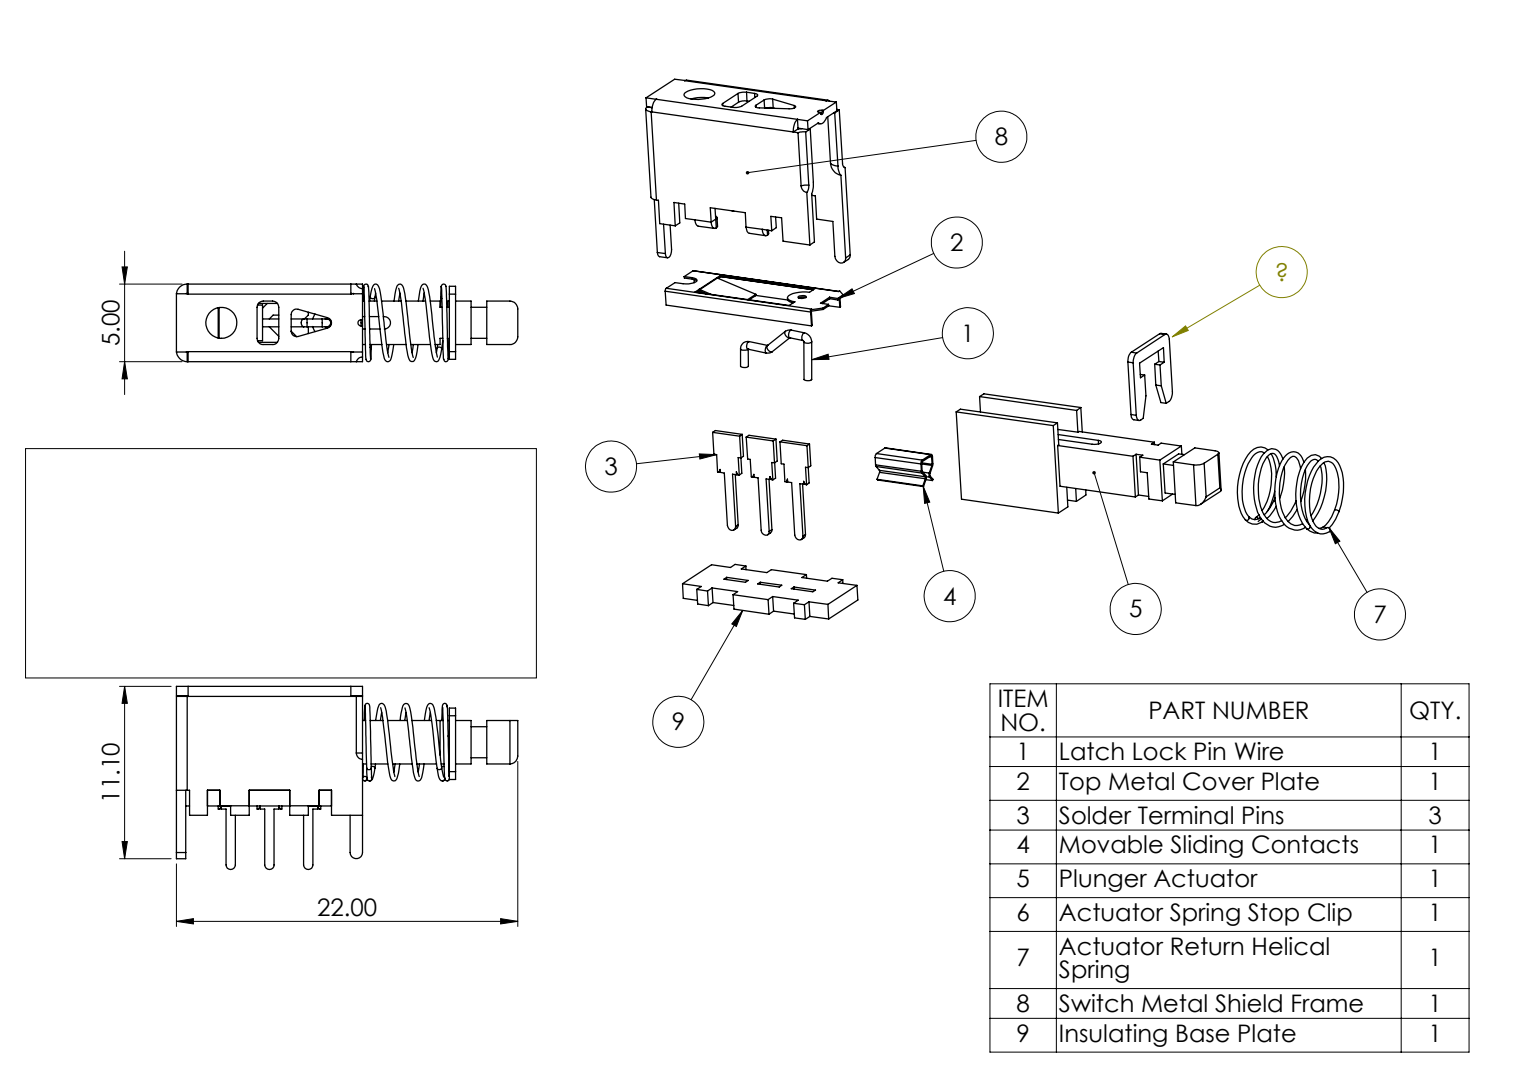
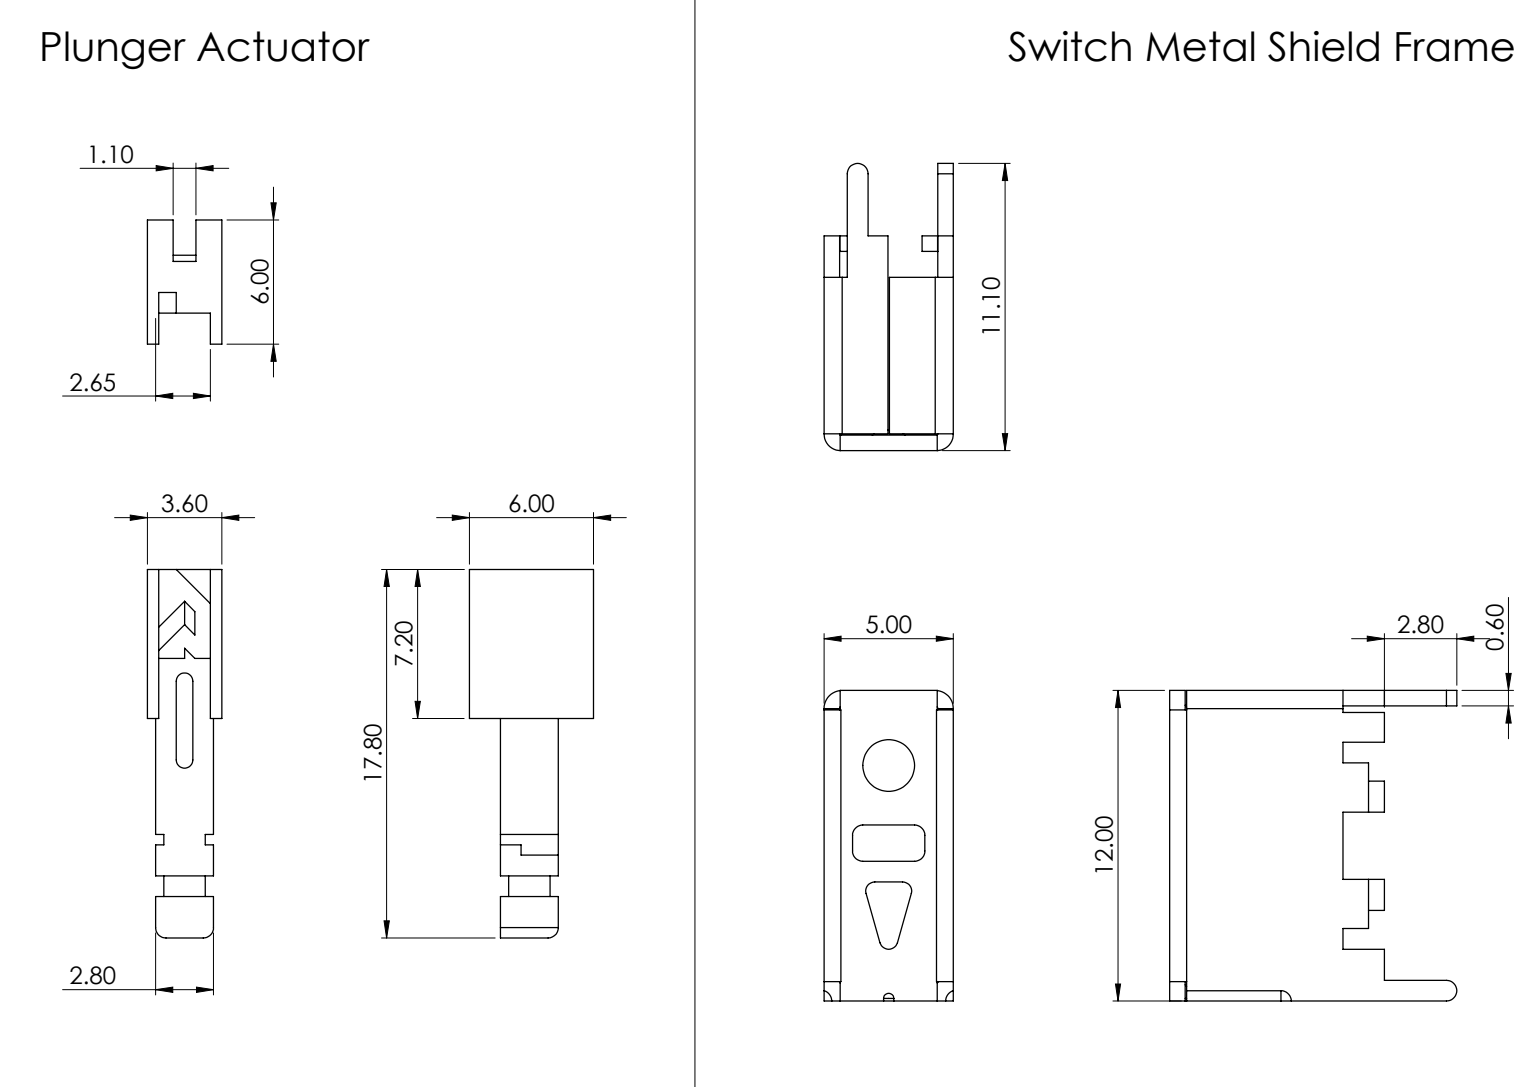
ISO-10303-21;
HEADER;
FILE_DESCRIPTION (('STEP AP214'),
    '1' );
FILE_NAME ('MAS-687',
    '2026-10-09T19:32:29',
    ( '' ),
    ( '' ),
    'SwSTEP 2.0',
    'SolidWorks 2026',
    '' );
FILE_SCHEMA (( 'AUTOMOTIVE_DESIGN' ));
ENDSEC;

DATA;
#1 = PRODUCT_DEFINITION_FORMATION_WITH_SPECIFIED_SOURCE ( 'ANY', '', #17748, .NOT_KNOWN. ) ;
#2 = ORIENTED_EDGE ( 'NONE', *, *, #12081, .F. ) ;
#3 = CARTESIAN_POINT ( 'NONE',  ( -1.670747221194380128, -5.103620102360550526, 3.047345349617600174 ) ) ;
#4 = SURFACE_STYLE_USAGE ( .BOTH. , #13787 ) ;
#5 = CARTESIAN_POINT ( 'NONE',  ( 1.315859850362970151, -5.328211948015590060, 2.737664967889629875 ) ) ;
#6 = VECTOR ( 'NONE', #12765, 1000.000000000000000 ) ;
#7 = CARTESIAN_POINT ( 'NONE',  ( 0.1749999999999999889, 2.700000000000000178, 0.5999999999999999778 ) ) ;
#8 = CARTESIAN_POINT ( 'NONE',  ( -0.4005155088301869948, -1.125163681423230200, 7.019123328904779413 ) ) ;
#9 = CYLINDRICAL_SURFACE ( 'NONE', #17623, 0.01000000000000002623 ) ;
#10 = CARTESIAN_POINT ( 'NONE',  ( -0.8934014991059870958, -4.614566048306490309, 6.877287176483410924 ) ) ;
#11 = DIRECTION ( 'NONE',  ( 1.306144734853129823E-16, -1.000000000000000000, -1.306144734853129823E-16 ) ) ;
#12 = CARTESIAN_POINT ( 'NONE',  ( 2.044452488559148851, -4.148800282540726414, 4.887392274793745273 ) ) ;
#13 = EDGE_CURVE ( 'NONE', #12197, #10130, #5306, .T. ) ;
#14 = CARTESIAN_POINT ( 'NONE',  ( -7.186903215246500006E-16, 5.131370849898470254, 6.100000000000000533 ) ) ;
#15 = EDGE_LOOP ( 'NONE', ( #13196, #1670, #3615, #581 ) ) ;
#16 = CYLINDRICAL_SURFACE ( 'NONE', #2043, 0.04999999999999969746 ) ;
#17 = EDGE_LOOP ( 'NONE', ( #524, #5810, #763, #9068 ) ) ;
#18 = CYLINDRICAL_SURFACE ( 'NONE', #7513, 0.2500000000000002220 ) ;
#19 = ORIENTED_EDGE ( 'NONE', *, *, #12813, .F. ) ;
#20 = CIRCLE ( 'NONE', #8305, 0.5000000000000000000 ) ;
#21 = CARTESIAN_POINT ( 'NONE',  ( -1.250000000000000000, 0.5999999999999999778, 7.599999999999999645 ) ) ;
#22 = EDGE_LOOP ( 'NONE', ( #588, #1750, #4383 ) ) ;
#23 = CARTESIAN_POINT ( 'NONE',  ( -1.526871680339578541, -5.259957627118655665, 3.327650196883449762 ) ) ;
#24 = CARTESIAN_POINT ( 'NONE',  ( 1.236224677598260158, -1.986830348089900777, 2.351625617688071657 ) ) ;
#25 = CARTESIAN_POINT ( 'NONE',  ( 0.3750000000000000000, 6.450000000000000178, 2.100000000000000089 ) ) ;
#26 = CARTESIAN_POINT ( 'NONE',  ( 1.652654650382400003, -0.7952867690272209522, 3.029252778805629820 ) ) ;
#27 = DIRECTION ( 'NONE',  ( 0.000000000000000000, 0.000000000000000000, -1.000000000000000000 ) ) ;
#28 = CARTESIAN_POINT ( 'NONE',  ( 0.5500000000000000444, 2.050000000000000266, 1.600000000000000089 ) ) ;
#29 = CARTESIAN_POINT ( 'NONE',  ( 1.850000000000000089, -5.599999999999999645, 6.400000000000000355 ) ) ;
#30 = AXIS2_PLACEMENT_3D ( 'NONE', #13757, #16263, #2391 ) ;
#31 = CARTESIAN_POINT ( 'NONE',  ( -1.669205944673819886, -3.147403886144329643, 6.359065158982450505 ) ) ;
#32 = CARTESIAN_POINT ( 'NONE',  ( -1.599895119336340876, -2.871785303044851023, 5.986560317183706736 ) ) ;
#33 = CARTESIAN_POINT ( 'NONE',  ( 1.821706171509118954, -0.09788135593220394226, 5.646608543709396244 ) ) ;
#34 = EDGE_CURVE ( 'NONE', #13183, #12938, #7797, .T. ) ;
#35 = CARTESIAN_POINT ( 'NONE',  ( -0.06264882350515391107, -0.4512711864406790396, 7.052569299041220319 ) ) ;
#36 = PLANE ( 'NONE',  #7974 ) ;
#37 = VERTEX_POINT ( 'NONE', #9466 ) ;
#38 = CARTESIAN_POINT ( 'NONE',  ( -2.058670345754650022, -0.2491525423728820077, 3.559656372813929881 ) ) ;
#39 = CARTESIAN_POINT ( 'NONE',  ( -0.09706517602693919000, -2.961097579838030125, 7.051451474958980725 ) ) ;
#40 = ORIENTED_EDGE ( 'NONE', *, *, #16715, .F. ) ;
#41 = DIRECTION ( 'NONE',  ( -0.7049180327868849183, 0.7092887755011130224, 8.531426931033447850E-16 ) ) ;
#42 = ORIENTED_EDGE ( 'NONE', *, *, #5974, .F. ) ;
#43 = CARTESIAN_POINT ( 'NONE',  ( 2.062913653388429136, -2.382731248990799688, 5.832754583370791224 ) ) ;
#44 = AXIS2_PLACEMENT_3D ( 'NONE', #5027, #10483, #9189 ) ;
#45 =( NAMED_UNIT ( * ) SI_UNIT ( $, .STERADIAN. ) SOLID_ANGLE_UNIT ( ) );
#46 = CARTESIAN_POINT ( 'NONE',  ( -0.6640878839024662028, -5.462076271186444565, 7.269405042592523181 ) ) ;
#47 = ORIENTED_EDGE ( 'NONE', *, *, #18282, .T. ) ;
#48 = CARTESIAN_POINT ( 'NONE',  ( 0.7109160811436110450, -1.307629111369560171, 6.943511536198400336 ) ) ;
#49 = CARTESIAN_POINT ( 'NONE',  ( 1.750316316486830059, -0.3400423728813560253, 3.126818518378580158 ) ) ;
#50 = EDGE_LOOP ( 'NONE', ( #8387, #9597, #10554, #1667 ) ) ;
#51 = PLANE ( 'NONE',  #9042 ) ;
#52 = DIRECTION ( 'NONE',  ( -2.379049338482479710E-16, 0.000000000000000000, -1.000000000000000000 ) ) ;
#53 = CARTESIAN_POINT ( 'NONE',  ( -1.883235269974520287, -3.240557039297494057, 5.517512544583926370 ) ) ;
#54 = CARTESIAN_POINT ( 'NONE',  ( 0.5500000000000000444, 6.450000000000000178, 3.399999999999999911 ) ) ;
#55 = ORIENTED_EDGE ( 'NONE', *, *, #7049, .T. ) ;
#56 = PLANE ( 'NONE',  #5985 ) ;
#57 = DIRECTION ( 'NONE',  ( 0.000000000000000000, 6.123233995736769734E-17, -1.000000000000000000 ) ) ;
#58 = CARTESIAN_POINT ( 'NONE',  ( 0.5137283630188955730, -0.4379237288135597317, 6.687652957477222770 ) ) ;
#59 = EDGE_LOOP ( 'NONE', ( #2998, #8111, #2641, #14217 ) ) ;
#60 = CARTESIAN_POINT ( 'NONE',  ( -1.440522616026439495, -4.804713230972779137, 3.241384813161591438 ) ) ;
#61 = CARTESIAN_POINT ( 'NONE',  ( -1.647941990407690627, -5.555508474576275724, 3.475676388127094896 ) ) ;
#62 = ORIENTED_EDGE ( 'NONE', *, *, #5567, .F. ) ;
#63 = FACE_OUTER_BOUND ( 'NONE', #13945, .T. ) ;
#64 = DIRECTION ( 'NONE',  ( 1.000000000000000000, 0.000000000000000000, 0.000000000000000000 ) ) ;
#65 = CARTESIAN_POINT ( 'NONE',  ( -0.5198535559317755128, -0.5906145504024216120, 2.087183161631441131 ) ) ;
#66 = ORIENTED_EDGE ( 'NONE', *, *, #5755, .T. ) ;
#67 = LINE ( 'NONE', #9878, #10862 ) ;
#68 = CARTESIAN_POINT ( 'NONE',  ( 1.097561405233190124, -1.986830348089889897, 2.618148744692249785 ) ) ;
#69 = FACE_OUTER_BOUND ( 'NONE', #15642, .T. ) ;
#70 = CARTESIAN_POINT ( 'NONE',  ( -2.039016451601939117, -3.011515032774579215, 4.939402908764104261 ) ) ;
#71 = LINE ( 'NONE', #1553, #14401 ) ;
#72 = ORIENTED_EDGE ( 'NONE', *, *, #16562, .F. ) ;
#73 = COLOUR_RGB ( '', 0.09019608, 0.27058824, 0.51372549) ;
#74 = CARTESIAN_POINT ( 'NONE',  ( 0.5500000000000000444, 6.450000000000000178, 3.200000000000000178 ) ) ;
#75 = CARTESIAN_POINT ( 'NONE',  ( -0.5609751937345790473, -0.4601694915254239682, 7.293870047334757523 ) ) ;
#76 = CARTESIAN_POINT ( 'NONE',  ( -1.145304265383870090, -3.077539021279469988, 6.755972720436099088 ) ) ;
#77 = LINE ( 'NONE', #14322, #1274 ) ;
#78 = LINE ( 'NONE', #15272, #17717 ) ;
#79 = CARTESIAN_POINT ( 'NONE',  ( -2.638803263991410741, -5.219915254237295521, 4.982085668537435730 ) ) ;
#80 = ORIENTED_EDGE ( 'NONE', *, *, #2571, .F. ) ;
#81 = ORIENTED_EDGE ( 'NONE', *, *, #13193, .F. ) ;
#82 = CARTESIAN_POINT ( 'NONE',  ( 2.500000000000000000, 10.00000000000000000, 1.600000000000000089 ) ) ;
#83 = DIRECTION ( 'NONE',  ( -1.000000000000000000, 0.000000000000000000, 0.000000000000000000 ) ) ;
#84 = VERTEX_POINT ( 'NONE', #15129 ) ;
#85 = CARTESIAN_POINT ( 'NONE',  ( 1.668426559427239608, -1.214475958216409746, 6.763847501342977075 ) ) ;
#86 = EDGE_CURVE ( 'NONE', #1835, #616, #17602, .T. ) ;
#87 = FILL_AREA_STYLE ('',( #1375 ) ) ;
#88 = AXIS2_PLACEMENT_3D ( 'NONE', #12369, #6813, #17991 ) ;
#89 = CARTESIAN_POINT ( 'NONE',  ( 0.2435295127647320035, -5.004947479095229745, 2.350795284704489507 ) ) ;
#90 = EDGE_CURVE ( 'NONE', #4403, #2448, #5018, .T. ) ;
#91 = LINE ( 'NONE', #17013, #9613 ) ;
#92 = CARTESIAN_POINT ( 'NONE',  ( -1.026235786675429917, -1.195028546288090077, 6.817920158464570335 ) ) ;
#93 = EDGE_CURVE ( 'NONE', #12376, #4659, #13727, .T. ) ;
#94 = LINE ( 'NONE', #11471, #11442 ) ;
#95 = CARTESIAN_POINT ( 'NONE',  ( 0.6150581927482109412, -4.451548030288480895, 6.971662190339319665 ) ) ;
#96 = DIRECTION ( 'NONE',  ( 6.123233995736769734E-17, 0.000000000000000000, 1.000000000000000000 ) ) ;
#97 = CARTESIAN_POINT ( 'NONE',  ( 0.8893259633308030487, -3.846052534792983923, 2.849594321892129134 ) ) ;
#98 = DIRECTION ( 'NONE',  ( -2.220446049250309876E-16, 1.000000000000000000, 0.000000000000000000 ) ) ;
#99 = ORIENTED_EDGE ( 'NONE', *, *, #10473, .T. ) ;
#100 = DIRECTION ( 'NONE',  ( 1.306144734853129823E-16, -1.000000000000000000, -1.306144734853129823E-16 ) ) ;
#101 = ORIENTED_EDGE ( 'NONE', *, *, #7303, .T. ) ;
#102 = DIRECTION ( 'NONE',  ( 0.7071067811865480168, 0.7071067811865470176, 0.000000000000000000 ) ) ;
#103 = VERTEX_POINT ( 'NONE', #12339 ) ;
#104 = CARTESIAN_POINT ( 'NONE',  ( -1.000000000000000000, -5.000000000000000000, 6.100000000000000533 ) ) ;
#105 = ADVANCED_FACE ( 'NONE', ( #14933 ), #6784, .T. ) ;
#106 = ORIENTED_EDGE ( 'NONE', *, *, #2225, .T. ) ;
#107 = CARTESIAN_POINT ( 'NONE',  ( -1.489797906646480596, -5.188771186440680694, 6.112509577910826941 ) ) ;
#108 = EDGE_CURVE ( 'NONE', #9178, #84, #9359, .T. ) ;
#109 = DIRECTION ( 'NONE',  ( -1.000000000000000000, 0.000000000000000000, 0.000000000000000000 ) ) ;
#110 = CARTESIAN_POINT ( 'NONE',  ( 2.500000000000000000, 11.15000000000000036, -1.135674796306499891E-15 ) ) ;
#111 = EDGE_CURVE ( 'NONE', #2785, #786, #2714, .T. ) ;
#112 = CARTESIAN_POINT ( 'NONE',  ( 1.889999999999999902, 7.299999999999999822, 0.5999999999999999778 ) ) ;
#113 = CARTESIAN_POINT ( 'NONE',  ( 2.500000000000000000, 2.000000000000000000, 1.600000000000000089 ) ) ;
#114 = DIRECTION ( 'NONE',  ( 0.000000000000000000, -1.000000000000000000, 0.000000000000000000 ) ) ;
#115 = CARTESIAN_POINT ( 'NONE',  ( -1.000000000000000000, -5.000000000000000000, 6.100000000000000533 ) ) ;
#116 = CARTESIAN_POINT ( 'NONE',  ( -0.09706517602693919000, -2.961097579838030125, 7.051451474958980725 ) ) ;
#117 = CARTESIAN_POINT ( 'NONE',  ( 1.978802102381368888, -3.756740257999804378, 4.152967933079626306 ) ) ;
#118 = CARTESIAN_POINT ( 'NONE',  ( 1.851073041990159984, -0.4067796610169499560, 6.153284478378259870 ) ) ;
#119 = PLANE ( 'NONE',  #9386 ) ;
#120 = DIRECTION ( 'NONE',  ( -0.000000000000000000, 1.000000000000000000, 0.000000000000000000 ) ) ;
#121 = ORIENTED_EDGE ( 'NONE', *, *, #17653, .F. ) ;
#122 = CARTESIAN_POINT ( 'NONE',  ( 0.3803919826356921829, -0.008898305084746057844, 2.682580100125298461 ) ) ;
#123 = CARTESIAN_POINT ( 'NONE',  ( -1.552749016687749783, -1.563800282540730002, 6.468535037441760061 ) ) ;
#124 = ORIENTED_EDGE ( 'NONE', *, *, #9369, .T. ) ;
#125 = ORIENTED_EDGE ( 'NONE', *, *, #6265, .F. ) ;
#126 = CARTESIAN_POINT ( 'NONE',  ( 1.236334101859160262, -3.570433951693499974, 2.697445712080690949 ) ) ;
#127 = DIRECTION ( 'NONE',  ( 1.000000000000000000, 0.000000000000000000, 0.000000000000000000 ) ) ;
#128 = CARTESIAN_POINT ( 'NONE',  ( -2.560337424259679917, -5.537711864406785978, 4.001768473655595848 ) ) ;
#129 = EDGE_CURVE ( 'NONE', #14329, #8376, #6958, .T. ) ;
#130 = ORIENTED_EDGE ( 'NONE', *, *, #2305, .T. ) ;
#131 = CARTESIAN_POINT ( 'NONE',  ( -1.432215783582709401, -0.4868644067796619179, 6.170863372171116801 ) ) ;
#132 = EDGE_LOOP ( 'NONE', ( #12967, #8164, #8169, #17199, #14235, #13899, #10080, #12493, #3954, #15631, #1582, #17423, #1346, #16815, #17146, #660 ) ) ;
#133 = PLANE ( 'NONE',  #14387 ) ;
#134 = DIRECTION ( 'NONE',  ( 0.000000000000000000, 1.000000000000000000, -2.081668171172166936E-15 ) ) ;
#135 = VECTOR ( 'NONE', #8879, 1000.000000000000000 ) ;
#136 = CARTESIAN_POINT ( 'NONE',  ( 1.854389246811829706, -2.448755237495690462, 3.819010576716856065 ) ) ;
#137 = CARTESIAN_POINT ( 'NONE',  ( 2.638803263991410741, -0.3800847457627119508, 4.982085668537405532 ) ) ;
#138 = VERTEX_POINT ( 'NONE', #2989 ) ;
#139 = LINE ( 'NONE', #14116, #7062 ) ;
#140 = CARTESIAN_POINT ( 'NONE',  ( 1.965557623688110933, -0.3889830508474575455, 5.292675575926325315 ) ) ;
#141 = ORIENTED_EDGE ( 'NONE', *, *, #4492, .T. ) ;
#142 = ORIENTED_EDGE ( 'NONE', *, *, #9998, .T. ) ;
#143 = DIRECTION ( 'NONE',  ( 0.000000000000000000, -1.000000000000000000, -1.306144734853125878E-16 ) ) ;
#144 = CARTESIAN_POINT ( 'NONE',  ( 0.05465110135556765225, -5.448728813559320372, 6.752241303418941243 ) ) ;
#145 = CARTESIAN_POINT ( 'NONE',  ( 2.011500846714318502, -0.04894067796610199889, 3.478373409938461336 ) ) ;
#146 = CARTESIAN_POINT ( 'NONE',  ( 1.791574935211219799, -5.408686440677969998, 6.226029630577610163 ) ) ;
#147 = CARTESIAN_POINT ( 'NONE',  ( -0.2097343361107079085, -0.5962015548080615845, 2.050670208512068715 ) ) ;
#148 = EDGE_CURVE ( 'NONE', #7436, #747, #4086, .T. ) ;
#149 = ORIENTED_EDGE ( 'NONE', *, *, #14001, .F. ) ;
#150 = CARTESIAN_POINT ( 'NONE',  ( 1.917298190932609891, -2.103271789531340197, 3.335187436117899917 ) ) ;
#151 = VECTOR ( 'NONE', #14058, 1000.000000000000000 ) ;
#152 = DIRECTION ( 'NONE',  ( 5.887846720064179370E-16, 1.000000000000000000, 0.000000000000000000 ) ) ;
#153 = CARTESIAN_POINT ( 'NONE',  ( -1.831349212334698828, -1.590929447188999646, 3.772065786216939554 ) ) ;
#154 = CYLINDRICAL_SURFACE ( 'NONE', #14694, 0.6500000000000003553 ) ;
#155 = EDGE_CURVE ( 'NONE', #7849, #17929, #15593, .T. ) ;
#156 = ORIENTED_EDGE ( 'NONE', *, *, #7147, .T. ) ;
#157 = CARTESIAN_POINT ( 'NONE',  ( 1.899999999999999911, 4.700000000000000178, 1.600000000000000089 ) ) ;
#158 = CARTESIAN_POINT ( 'NONE',  ( -2.020286629067959971, -0.4913135593220345210, 6.420841923842841581 ) ) ;
#159 = CARTESIAN_POINT ( 'NONE',  ( -2.283153923255329953, -3.403575057315510133, 4.129076318403500423 ) ) ;
#160 = CARTESIAN_POINT ( 'NONE',  ( -2.350000000000000089, -5.599999999999999645, 6.400000000000000355 ) ) ;
#161 = DIRECTION ( 'NONE',  ( 5.551115123125780730E-16, 1.000000000000000000, 0.000000000000000000 ) ) ;
#162 = CARTESIAN_POINT ( 'NONE',  ( -2.458531667407850563, -5.206567796610170440, 5.699238225248945966 ) ) ;
#163 = ORIENTED_EDGE ( 'NONE', *, *, #9591, .T. ) ;
#164 = EDGE_LOOP ( 'NONE', ( #16318, #961, #5589, #9306 ) ) ;
#165 = CARTESIAN_POINT ( 'NONE',  ( -2.353194804772640314, -5.224364406779659298, 4.731327187377240229 ) ) ;
#166 = DIRECTION ( 'NONE',  ( 1.000000000000000000, 1.306144734853129823E-16, 0.000000000000000000 ) ) ;
#167 = ORIENTED_EDGE ( 'NONE', *, *, #2479, .T. ) ;
#168 = CARTESIAN_POINT ( 'NONE',  ( -2.349129089426440054, -4.894025507765950245, 4.842612091679129982 ) ) ;
#169 = VECTOR ( 'NONE', #1507, 1000.000000000000000 ) ;
#170 = CARTESIAN_POINT ( 'NONE',  ( 0.6575972843460591299, -0.3612150962701959900, 2.110392115010549130 ) ) ;
#171 = CARTESIAN_POINT ( 'NONE',  ( 0.9000000000000000222, -10.00000000000000000, 6.100000000000000533 ) ) ;
#172 = CARTESIAN_POINT ( 'NONE',  ( 2.334032080503399609, -2.289578095837639715, 5.001728246382190157 ) ) ;
#173 = ADVANCED_FACE ( 'NONE', ( #18226 ), #12517, .F. ) ;
#174 = CARTESIAN_POINT ( 'NONE',  ( 1.889999999999999902, 8.500000000000000000, 0.5999999999999999778 ) ) ;
#175 = CARTESIAN_POINT ( 'NONE',  ( 1.724579595320000047, -3.939205687946140344, 3.098572228637889836 ) ) ;
#176 = DIRECTION ( 'NONE',  ( 1.000000000000000000, 0.000000000000000000, 0.000000000000000000 ) ) ;
#177 = EDGE_CURVE ( 'NONE', #9615, #14727, #5673, .T. ) ;
#178 = CARTESIAN_POINT ( 'NONE',  ( 1.835037444103841286, -4.241953435693877061, 5.620619042473564697 ) ) ;
#179 = CARTESIAN_POINT ( 'NONE',  ( -1.000000000000000000, 6.400000000000000355, 7.700000000000000178 ) ) ;
#180 = CARTESIAN_POINT ( 'NONE',  ( 2.011500846714319835, -0.3489406779661020086, 3.478373409938460448 ) ) ;
#181 = ORIENTED_EDGE ( 'NONE', *, *, #15801, .T. ) ;
#182 = CARTESIAN_POINT ( 'NONE',  ( -1.899999999999999911, 7.299999999999999822, 0.6099999999999999867 ) ) ;
#183 = ORIENTED_EDGE ( 'NONE', *, *, #8245, .T. ) ;
#184 = AXIS2_PLACEMENT_3D ( 'NONE', #11103, #16750, #840 ) ;
#185 = ADVANCED_FACE ( 'NONE', ( #9836 ), #11122, .T. ) ;
#186 = ORIENTED_EDGE ( 'NONE', *, *, #6092, .T. ) ;
#187 = EDGE_CURVE ( 'NONE', #1492, #1173, #8443, .T. ) ;
#188 = CARTESIAN_POINT ( 'NONE',  ( -2.500000000000000000, 7.299999999999999822, 1.600000000000000089 ) ) ;
#189 = CARTESIAN_POINT ( 'NONE',  ( 1.899999999999999911, 9.199999999999999289, 1.600000000000000089 ) ) ;
#190 = ORIENTED_EDGE ( 'NONE', *, *, #14281, .T. ) ;
#191 = CARTESIAN_POINT ( 'NONE',  ( 1.782460458101500889, -5.399788135593215799, 5.718585207845976015 ) ) ;
#192 = CARTESIAN_POINT ( 'NONE',  ( -0.3832714063288900630, -2.685478996738538626, 7.326064873930687504 ) ) ;
#193 = CARTESIAN_POINT ( 'NONE',  ( -1.149999999999999911, 9.248236190979499227, 7.693185165257809821 ) ) ;
#194 = CARTESIAN_POINT ( 'NONE',  ( 1.662071288245189793, -0.7952852869591279239, 3.019836320359400084 ) ) ;
#195 = CARTESIAN_POINT ( 'NONE',  ( 1.899999999999999911, 0.5999999999999999778, 6.599999999999999645 ) ) ;
#196 = CARTESIAN_POINT ( 'NONE',  ( 0.009452110982653675123, -5.000192044704546035, 2.050000000000001155 ) ) ;
#197 = CLOSED_SHELL ( 'NONE', ( #3822, #8083, #11142, #1743, #2496, #9758, #12462, #15962, #6872, #9484, #17524, #17256, #4961, #15462, #764, #3248, #10059, #5969, #10152, #4929, #18252, #3273, #16322, #10513, #3922, #2712, #13996, #6295, #532, #11967, #9528, #2422, #10741, #3839, #15384, #3945, #14577, #1473, #15447, #8798, #14553, #6473, #731, #10373, #15290, #13653, #3441, #1008, #14533, #415, #7664, #14234 ) ) ;
#198 = AXIS2_PLACEMENT_3D ( 'NONE', #9946, #12907, #5782 ) ;
#199 = EDGE_CURVE ( 'NONE', #14776, #14634, #1931, .T. ) ;
#200 = FACE_OUTER_BOUND ( 'NONE', #10573, .T. ) ;
#201 = LINE ( 'NONE', #17127, #858 ) ;
#202 = CARTESIAN_POINT ( 'NONE',  ( 2.276802572547980130, -2.495331814072260013, 4.104251954998760610 ) ) ;
#203 = CARTESIAN_POINT ( 'NONE',  ( 1.750352751699790987, -3.686875393134939394, 3.627075451280439733 ) ) ;
#204 = CARTESIAN_POINT ( 'NONE',  ( 0.1910247150515120007, -0.004449152542373194588, 2.655937705488500722 ) ) ;
#205 = EDGE_CURVE ( 'NONE', #37, #8434, #9920, .T. ) ;
#206 = DIRECTION ( 'NONE',  ( 1.142876642996489981E-16, -1.000000000000000000, -6.530723674265629391E-17 ) ) ;
#207 = EDGE_CURVE ( 'NONE', #14363, #4874, #14274, .T. ) ;
#208 = VECTOR ( 'NONE', #15083, 1000.000000000000000 ) ;
#209 = CARTESIAN_POINT ( 'NONE',  ( 1.836970198721030057E-17, 2.299999999999999822, 7.700000000000000178 ) ) ;
#210 = ORIENTED_EDGE ( 'NONE', *, *, #3477, .T. ) ;
#211 = EDGE_CURVE ( 'NONE', #3339, #16796, #8542, .T. ) ;
#212 = CARTESIAN_POINT ( 'NONE',  ( -2.043308330018790198, -0.2002118644067800157, 5.867646457774669422 ) ) ;
#213 = CARTESIAN_POINT ( 'NONE',  ( -1.881914957835490121, -1.936412895153350133, 3.286797332666350435 ) ) ;
#214 = ORIENTED_EDGE ( 'NONE', *, *, #13, .F. ) ;
#215 = EDGE_CURVE ( 'NONE', #1195, #3917, #16867, .T. ) ;
#216 = EDGE_CURVE ( 'NONE', #16860, #6769, #9644, .T. ) ;
#217 = PLANE ( 'NONE',  #15934 ) ;
#218 = AXIS2_PLACEMENT_3D ( 'NONE', #8248, #6936, #4241 ) ;
#219 = ORIENTED_EDGE ( 'NONE', *, *, #701, .F. ) ;
#220 = VECTOR ( 'NONE', #13007, 1000.000000000000000 ) ;
#221 = CARTESIAN_POINT ( 'NONE',  ( -1.644832646965619372, -4.408812330071871344, 6.383232381746490880 ) ) ;
#222 = DIRECTION ( 'NONE',  ( 0.000000000000000000, 0.000000000000000000, 1.000000000000000000 ) ) ;
#223 = CARTESIAN_POINT ( 'NONE',  ( -2.645377369053839356, -5.228813559322024851, 4.488260618344918740 ) ) ;
#224 = CIRCLE ( 'NONE', #10856, 0.09999999999999939493 ) ;
#225 = ORIENTED_EDGE ( 'NONE', *, *, #4277, .F. ) ;
#226 = CIRCLE ( 'NONE', #1107, 0.3999999999999999667 ) ;
#227 = CARTESIAN_POINT ( 'NONE',  ( 2.270487904532159984, -0.3622881355932209835, 4.080813552109670894 ) ) ;
#228 = AXIS2_PLACEMENT_3D ( 'NONE', #7610, #10199, #579 ) ;
#229 = VERTEX_POINT ( 'NONE', #1406 ) ;
#230 = DIRECTION ( 'NONE',  ( -1.000000000000000000, 1.224646799147350002E-16, 0.000000000000000000 ) ) ;
#231 = CARTESIAN_POINT ( 'NONE',  ( 0.9000000000000000222, -10.00000000000000000, 3.799999999999999822 ) ) ;
#232 = B_SPLINE_CURVE_WITH_KNOTS ( 'NONE', 3,
 ( #17325, #2928, #4655, #4553, #14218, #1537, #7186 ),
 .UNSPECIFIED., .F., .F.,
 ( 4, 1, 1, 1, 4 ),
 ( 18.06415775814129887, 18.36448856483159986, 18.49670707487869947, 18.62179267666130045, 18.84955592153880133 ),
 .UNSPECIFIED. ) ;
#233 = CARTESIAN_POINT ( 'NONE',  ( 1.810994336139499783, -2.681638120378568857, 5.667058093962681120 ) ) ;
#234 = CARTESIAN_POINT ( 'NONE',  ( -1.850000000000000089, -6.000000000000000000, 2.799999999999999822 ) ) ;
#235 = VECTOR ( 'NONE', #9014, 1000.000000000000000 ) ;
#236 = ORIENTED_EDGE ( 'NONE', *, *, #9107, .F. ) ;
#237 = VECTOR ( 'NONE', #7753, 1000.000000000000000 ) ;
#238 = PLANE ( 'NONE',  #6124 ) ;
#239 = ADVANCED_FACE ( 'NONE', ( #1597 ), #11504, .T. ) ;
#240 = VERTEX_POINT ( 'NONE', #16423 ) ;
#241 = AXIS2_PLACEMENT_3D ( 'NONE', #8801, #14538, #6201 ) ;
#242 = DIRECTION ( 'NONE',  ( -1.000000000000000000, 1.480297366166879989E-15, 7.401486830834380223E-16 ) ) ;
#243 = CARTESIAN_POINT ( 'NONE',  ( -0.5664586606772434862, -5.586652542372875452, 2.726727161522279452 ) ) ;
#244 = APPLICATION_CONTEXT ( 'automotive_design' ) ;
#245 = CARTESIAN_POINT ( 'NONE',  ( 1.750000000000000000, 11.40000000000000036, 7.700000000000000178 ) ) ;
#246 = VECTOR ( 'NONE', #2226, 1000.000000000000000 ) ;
#247 = CARTESIAN_POINT ( 'NONE',  ( 1.000896394980339332, -0.1290254237288140371, 6.829956240957368863 ) ) ;
#248 = FACE_OUTER_BOUND ( 'NONE', #10929, .T. ) ;
#249 = AXIS2_PLACEMENT_3D ( 'NONE', #9297, #17801, #8028 ) ;
#250 = LINE ( 'NONE', #4404, #4362 ) ;
#251 = CARTESIAN_POINT ( 'NONE',  ( 0.03714311608463249925, -1.078587104846649991, 7.053160869216429596 ) ) ;
#252 = EDGE_CURVE ( 'NONE', #7890, #13271, #8186, .T. ) ;
#253 = DIRECTION ( 'NONE',  ( -1.000000000000000000, -1.168655815394900078E-16, -2.220446049250309876E-16 ) ) ;
#254 = CARTESIAN_POINT ( 'NONE',  ( -0.1086361371090530797, -2.662190708450249854, 6.750146344128172160 ) ) ;
#255 = VECTOR ( 'NONE', #13621, 1000.000000000000000 ) ;
#256 = AXIS2_PLACEMENT_3D ( 'NONE', #8428, #15667, #98 ) ;
#257 = DIRECTION ( 'NONE',  ( -1.189524669241239855E-16, 1.000000000000000000, 0.000000000000000000 ) ) ;
#258 = ORIENTED_EDGE ( 'NONE', *, *, #12874, .T. ) ;
#259 = ADVANCED_FACE ( 'NONE', ( #15058 ), #2172, .T. ) ;
#260 = VECTOR ( 'NONE', #17975, 1000.000000000000000 ) ;
#261 = CARTESIAN_POINT ( 'NONE',  ( -1.850000000000000089, -6.000000000000000000, 6.899999999999999467 ) ) ;
#262 = CARTESIAN_POINT ( 'NONE',  ( -2.321479326063761395, -0.5491525423728815802, 3.414080590619972710 ) ) ;
#263 = CARTESIAN_POINT ( 'NONE',  ( -0.2564439965878500538, -4.544701183441629766, 7.039440566481220074 ) ) ;
#264 = CARTESIAN_POINT ( 'NONE',  ( -1.899999999999999911, 7.299999999999999822, 1.600000000000000089 ) ) ;
#265 = DIRECTION ( 'NONE',  ( 0.000000000000000000, 0.000000000000000000, -1.000000000000000000 ) ) ;
#266 = CARTESIAN_POINT ( 'NONE',  ( -0.6640878839024662028, -5.162076271186444743, 7.269405042592523181 ) ) ;
#267 = ORIENTED_EDGE ( 'NONE', *, *, #17989, .T. ) ;
#268 = VERTEX_POINT ( 'NONE', #877 ) ;
#269 = LINE ( 'NONE', #7559, #15424 ) ;
#270 =( NAMED_UNIT ( * ) PLANE_ANGLE_UNIT ( ) SI_UNIT ( $, .RADIAN. ) );
#271 = DIRECTION ( 'NONE',  ( -1.000000000000000000, 3.700743415417179758E-16, 0.000000000000000000 ) ) ;
#272 = ORIENTED_EDGE ( 'NONE', *, *, #15142, .T. ) ;
#273 = CARTESIAN_POINT ( 'NONE',  ( -2.461935615161759294, -1.680241723982170754, 5.690952430644365734 ) ) ;
#274 = CARTESIAN_POINT ( 'NONE',  ( -0.009452110982655128821, -0.5998079552954630467, 2.350000000000000089 ) ) ;
#275 = DIRECTION ( 'NONE',  ( -1.000000000000000000, 0.000000000000000000, 0.000000000000000000 ) ) ;
#276 = CARTESIAN_POINT ( 'NONE',  ( 1.816660071039059909, -2.429307825567370127, 6.196159040268200968 ) ) ;
#277 = CARTESIAN_POINT ( 'NONE',  ( 1.338894208872951186, -5.333856471232010676, 3.139702328019969180 ) ) ;
#278 = CARTESIAN_POINT ( 'NONE',  ( 1.864786684738361178, -0.7952867690272195089, 2.817120744449660652 ) ) ;
#279 = VECTOR ( 'NONE', #3953, 1000.000000000000000 ) ;
#280 = DIRECTION ( 'NONE',  ( 1.850371707708589879E-16, 1.000000000000000000, 0.000000000000000000 ) ) ;
#281 = DIRECTION ( 'NONE',  ( 0.000000000000000000, 1.000000000000000000, 0.000000000000000000 ) ) ;
#282 = CARTESIAN_POINT ( 'NONE',  ( -1.953802435660519921, -4.987178660919110662, 4.069478085301024173 ) ) ;
#283 = FACE_OUTER_BOUND ( 'NONE', #8177, .T. ) ;
#284 = CARTESIAN_POINT ( 'NONE',  ( -6.735557395310430190E-17, 7.000000000000000000, 6.299999999999999822 ) ) ;
#285 = EDGE_LOOP ( 'NONE', ( #13386, #1128, #2, #3206 ) ) ;
#286 = LINE ( 'NONE', #5811, #9790 ) ;
#287 = ORIENTED_EDGE ( 'NONE', *, *, #878, .F. ) ;
#288 = CARTESIAN_POINT ( 'NONE',  ( -0.1749999999999999889, 5.200000000000000178, 1.600000000000000089 ) ) ;
#289 = DIRECTION ( 'NONE',  ( -1.110223024625160090E-15, -1.000000000000000000, 0.000000000000000000 ) ) ;
#290 = EDGE_LOOP ( 'NONE', ( #11237, #4760, #6614, #15056 ) ) ;
#291 = CIRCLE ( 'NONE', #11810, 0.4000000000000001887 ) ;
#292 = CARTESIAN_POINT ( 'NONE',  ( 0.2453710345350221533, -5.444279661016954819, 6.738252723719333481 ) ) ;
#293 = CARTESIAN_POINT ( 'NONE',  ( -2.339254516529639449, -2.918361879621429011, 5.953396186326395778 ) ) ;
#294 =( LENGTH_UNIT ( ) NAMED_UNIT ( * ) SI_UNIT ( .MILLI., .METRE. ) );
#295 = FILL_AREA_STYLE_COLOUR ( '', #15889 ) ;
#296 = CARTESIAN_POINT ( 'NONE',  ( 0.1749999999999999889, 8.800000000000000711, 0.4000000000000000222 ) ) ;
#297 = DIRECTION ( 'NONE',  ( 2.242874797222539596E-16, 1.794299837778029705E-15, 1.000000000000000000 ) ) ;
#298 = DIRECTION ( 'NONE',  ( -1.000000000000000000, 1.850371707708589879E-16, 7.401486830834380223E-16 ) ) ;
#299 = CARTESIAN_POINT ( 'NONE',  ( -2.036228139452650243, -3.473439922180369788, 3.519948877554409883 ) ) ;
#300 = CARTESIAN_POINT ( 'NONE',  ( 1.942813984510739056, -1.074746228486680000, 5.363608065214415355 ) ) ;
#301 = CARTESIAN_POINT ( 'NONE',  ( 0.5664586606772286093, -0.01334745762711899916, 2.726727161522279452 ) ) ;
#302 = LINE ( 'NONE', #16960, #1412 ) ;
#303 = AXIS2_PLACEMENT_3D ( 'NONE', #18184, #4318, #5723 ) ;
#304 = CARTESIAN_POINT ( 'NONE',  ( 1.550000000000000044, -5.599999999999999645, 6.100000000000000533 ) ) ;
#305 = VERTEX_POINT ( 'NONE', #7812 ) ;
#306 = CARTESIAN_POINT ( 'NONE',  ( 2.603140590302639890, -3.873181699441240244, 5.216500493824248963 ) ) ;
#307 = CARTESIAN_POINT ( 'NONE',  ( -0.7982439214406890082, -0.1690677966101698793, 6.591424794228156081 ) ) ;
#308 = CARTESIAN_POINT ( 'NONE',  ( 1.074829861819710075, -2.285737219477669946, 2.606322265575589991 ) ) ;
#309 = EDGE_LOOP ( 'NONE', ( #17351, #15970, #6172, #13800, #4182, #16945, #17442, #3306, #8429, #9460, #10234, #6980, #680, #8084, #3687, #8931, #1239, #12150, #7376, #3119, #7225, #7211, #16942, #5389, #10768, #17470, #4563, #16616 ) ) ;
#310 = ORIENTED_EDGE ( 'NONE', *, *, #13145, .F. ) ;
#311 = CARTESIAN_POINT ( 'NONE',  ( -1.444955263746759533, -3.267686203945749490, 2.842353646881510709 ) ) ;
#312 =( LENGTH_UNIT ( ) NAMED_UNIT ( * ) SI_UNIT ( .MILLI., .METRE. ) );
#313 = CARTESIAN_POINT ( 'NONE',  ( 2.651721837666119796, -5.073093220338980025, 4.594045830208265180 ) ) ;
#314 = ORIENTED_EDGE ( 'NONE', *, *, #15602, .T. ) ;
#315 = ADVANCED_FACE ( 'NONE', ( #5219 ), #2456, .T. ) ;
#316 = FACE_OUTER_BOUND ( 'NONE', #11871, .T. ) ;
#317 = AXIS2_PLACEMENT_3D ( 'NONE', #2282, #7935, #16259 ) ;
#318 = CARTESIAN_POINT ( 'NONE',  ( -2.350067830300900162, -0.5224576271186440746, 4.825253242917699303 ) ) ;
#319 = ORIENTED_EDGE ( 'NONE', *, *, #18192, .F. ) ;
#320 = EDGE_CURVE ( 'NONE', #15780, #4246, #13459, .T. ) ;
#321 = FACE_OUTER_BOUND ( 'NONE', #2353, .T. ) ;
#322 = EDGE_CURVE ( 'NONE', #6911, #16493, #5032, .T. ) ;
#323 = CARTESIAN_POINT ( 'NONE',  ( -0.1781895581254780980, -2.146007489747939090, 2.654724878163539969 ) ) ;
#324 = EDGE_CURVE ( 'NONE', #84, #12938, #3836, .T. ) ;
#325 = CARTESIAN_POINT ( 'NONE',  ( -1.713314936023349944, -0.5610169491525430763, 3.089913064446579760 ) ) ;
#326 = ORIENTED_EDGE ( 'NONE', *, *, #6822, .T. ) ;
#327 = FACE_OUTER_BOUND ( 'NONE', #394, .T. ) ;
#328 = DIRECTION ( 'NONE',  ( 1.000000000000000000, 1.224646799147350002E-16, 0.000000000000000000 ) ) ;
#329 = CARTESIAN_POINT ( 'NONE',  ( 1.289999999999999813, 7.900000000000002132, 3.000000000000002220 ) ) ;
#330 = EDGE_LOOP ( 'NONE', ( #3061, #9828, #5549, #10787 ) ) ;
#331 = VECTOR ( 'NONE', #11702, 1000.000000000000000 ) ;
#332 = CARTESIAN_POINT ( 'NONE',  ( 0.009303514085962454744, -0.3025471796894717014, 2.316528937223512497 ) ) ;
#333 = CARTESIAN_POINT ( 'NONE',  ( -1.088937603231280304, -5.573305084745765470, 2.959627624143549074 ) ) ;
#334 = CARTESIAN_POINT ( 'NONE',  ( 1.899999999999999911, 4.700000000000000178, 0.5999999999999999778 ) ) ;
#335 = CARTESIAN_POINT ( 'NONE',  ( 1.889999999999999902, 3.500000000000000000, -7.771561172376099727E-16 ) ) ;
#336 = B_SPLINE_CURVE_WITH_KNOTS ( 'NONE', 3,
 ( #3611, #846, #9261, #16396, #652, #10551, #6486, #16212, #12146, #3518, #17765, #8602, #2858, #12943, #14328, #1649 ),
 .UNSPECIFIED., .F., .F.,
 ( 4, 1, 1, 1, 1, 1, 1, 1, 1, 1, 1, 1, 1, 4 ),
 ( 0.4999998211434338868, 0.5106244842458940170, 0.5531978902117569152, 0.5957712970451829460, 0.6383447191101619955, 0.6809180289765489613, 0.7234918990886729517, 0.7660634153087889642, 0.8086437809560700352, 0.8511815656862139479, 0.8935997744640420404, 0.9363910903531720287, 0.9718312009676199903, 1.000000000000000000 ),
 .UNSPECIFIED. ) ;
#337 = CARTESIAN_POINT ( 'NONE',  ( -1.236224677598320332, -3.613169651910099756, 2.351625617688101411 ) ) ;
#338 = ORIENTED_EDGE ( 'NONE', *, *, #2122, .F. ) ;
#339 = CARTESIAN_POINT ( 'NONE',  ( -1.219286470748949913, -1.218316834576380181, 6.712979431025680732 ) ) ;
#340 = EDGE_CURVE ( 'NONE', #11433, #9105, #9389, .T. ) ;
#341 = FACE_OUTER_BOUND ( 'NONE', #1960, .T. ) ;
#342 = CARTESIAN_POINT ( 'NONE',  ( 2.029711248330070994, -2.219713230972778728, 4.391497016172514201 ) ) ;
#343 = CARTESIAN_POINT ( 'NONE',  ( -6.735557395310420329E-17, 6.700000000000000178, 6.299999999999999822 ) ) ;
#344 = DIRECTION ( 'NONE',  ( 1.708035422500239940E-16, 1.000000000000000000, 5.978123978750840407E-16 ) ) ;
#345 = ORIENTED_EDGE ( 'NONE', *, *, #10185, .F. ) ;
#346 = CARTESIAN_POINT ( 'NONE',  ( -1.250000000000000000, 0.5999999999999999778, 6.100000000000000533 ) ) ;
#347 = CARTESIAN_POINT ( 'NONE',  ( 2.524473153133520054, -0.6128213390808875394, 3.881373716577345867 ) ) ;
#348 = CARTESIAN_POINT ( 'NONE',  ( -0.8934014991059870958, -4.614566048306490309, 6.877287176483410924 ) ) ;
#349 = CARTESIAN_POINT ( 'NONE',  ( -1.800000000000000044, 11.40000000000000036, 7.649999999999999467 ) ) ;
#350 = CARTESIAN_POINT ( 'NONE',  ( 1.850000000000000089, 0.7500000000000000000, 7.649999999999999467 ) ) ;
#351 = CARTESIAN_POINT ( 'NONE',  ( 2.351526912647309953, -5.073093220338979137, 4.606040641882800379 ) ) ;
#352 = EDGE_LOOP ( 'NONE', ( #6999, #6754, #2770, #1267 ) ) ;
#353 = ORIENTED_EDGE ( 'NONE', *, *, #5292, .T. ) ;
#354 = DIRECTION ( 'NONE',  ( 0.000000000000000000, 0.000000000000000000, 1.000000000000000000 ) ) ;
#355 = PLANE ( 'NONE',  #1395 ) ;
#356 = VERTEX_POINT ( 'NONE', #17700 ) ;
#357 = CARTESIAN_POINT ( 'NONE',  ( -1.149999999999999911, 9.274118095489749081, 7.596592582628910684 ) ) ;
#358 = CARTESIAN_POINT ( 'NONE',  ( 2.022685914314938938, -1.167899381639830203, 6.418096442297061444 ) ) ;
#359 = EDGE_CURVE ( 'NONE', #3082, #8454, #16331, .T. ) ;
#360 = CARTESIAN_POINT ( 'NONE',  ( 1.139503474074560874, -0.7471169921413568504, 2.982738323988489260 ) ) ;
#361 = CARTESIAN_POINT ( 'NONE',  ( 1.899999999999999911, 2.799999999999999822, 1.600000000000000089 ) ) ;
#362 = CARTESIAN_POINT ( 'NONE',  ( -0.3413183941262150078, -2.685478996738539958, 7.028571974690709823 ) ) ;
#363 = CARTESIAN_POINT ( 'NONE',  ( -0.02999999999999379899, 12.00000000000000000, -2.869354249208270301E-17 ) ) ;
#364 = CARTESIAN_POINT ( 'NONE',  ( -0.1785884594054470975, -1.400782264522720366, 7.347870815423047652 ) ) ;
#365 = CARTESIAN_POINT ( 'NONE',  ( 1.899999999999999911, 7.299999999999999822, 0.6099999999999999867 ) ) ;
#366 = CARTESIAN_POINT ( 'NONE',  ( 0.1608173401625761778, -4.498124606865046893, 6.746714348835997299 ) ) ;
#367 = CARTESIAN_POINT ( 'NONE',  ( -2.043308330018790198, -0.5002118644067800046, 5.867646457774669422 ) ) ;
#368 = LINE ( 'NONE', #14, #4331 ) ;
#369 = CARTESIAN_POINT ( 'NONE',  ( 0.1749999999999999889, 7.500000000000000000, 3.100000000000000089 ) ) ;
#370 = ORIENTED_EDGE ( 'NONE', *, *, #6530, .F. ) ;
#371 = DIRECTION ( 'NONE',  ( -1.000000000000000000, 0.000000000000000000, 0.000000000000000000 ) ) ;
#372 = EDGE_LOOP ( 'NONE', ( #10666, #14825, #6919, #6474 ) ) ;
#373 = PLANE ( 'NONE',  #10593 ) ;
#374 = EDGE_LOOP ( 'NONE', ( #16981, #5498, #13083, #14749 ) ) ;
#375 = VECTOR ( 'NONE', #12826, 1000.000000000000000 ) ;
#376 = CARTESIAN_POINT ( 'NONE',  ( -3.503171016405825766E-15, -5.300000000000000711, 2.649999999999998579 ) ) ;
#377 = CARTESIAN_POINT ( 'NONE',  ( -2.353343516942199898, -1.773394877135329839, 4.722803042560189901 ) ) ;
#378 = CARTESIAN_POINT ( 'NONE',  ( 0.4722227023514015687, -3.477280798540335560, 2.088464165977070408 ) ) ;
#379 = EDGE_CURVE ( 'NONE', #14325, #1999, #10215, .T. ) ;
#380 = PRESENTATION_STYLE_ASSIGNMENT (( #14351 ) ) ;
#381 =( NAMED_UNIT ( * ) SI_UNIT ( $, .STERADIAN. ) SOLID_ANGLE_UNIT ( ) );
#382 = DIRECTION ( 'NONE',  ( 1.000000000000000000, 0.000000000000000000, 0.000000000000000000 ) ) ;
#383 = CARTESIAN_POINT ( 'NONE',  ( 1.928817277882869829, -1.144611093351550091, 6.048484184565929844 ) ) ;
#384 = CARTESIAN_POINT ( 'NONE',  ( -1.600000000000000089, -3.475292999508519705E-16, 4.000000000000000000 ) ) ;
#385 = CARTESIAN_POINT ( 'NONE',  ( 1.401708661791409849, -4.358394877135329359, 6.590491606684049763 ) ) ;
#386 = CARTESIAN_POINT ( 'NONE',  ( -2.032257487115171291, -4.571830348089889640, 4.991258216523934976 ) ) ;
#387 = CARTESIAN_POINT ( 'NONE',  ( 0.009037091307169229856, -5.006769755134070188, 2.399753621991540076 ) ) ;
#388 = FACE_OUTER_BOUND ( 'NONE', #11566, .T. ) ;
#389 = VERTEX_POINT ( 'NONE', #1060 ) ;
#390 = CARTESIAN_POINT ( 'NONE',  ( 2.543624461644950152, -3.896469987729531681, 5.457025951419980814 ) ) ;
#391 = CARTESIAN_POINT ( 'NONE',  ( -2.051331987628511211, -0.2269067796610169385, 4.618035453557344461 ) ) ;
#392 = CARTESIAN_POINT ( 'NONE',  ( -2.111627294540180166, -1.889836318576769925, 3.660877362176710559 ) ) ;
#393 = ORIENTED_EDGE ( 'NONE', *, *, #5976, .T. ) ;
#394 = EDGE_LOOP ( 'NONE', ( #11957, #9883, #11083, #12392 ) ) ;
#395 = FACE_OUTER_BOUND ( 'NONE', #17771, .T. ) ;
#396 = VERTEX_POINT ( 'NONE', #6700 ) ;
#397 = CARTESIAN_POINT ( 'NONE',  ( 1.741913176380120110, -3.640298816558360517, 3.117443785062520067 ) ) ;
#398 = EDGE_CURVE ( 'NONE', #13449, #7267, #12359, .T. ) ;
#399 = SHAPE_DEFINITION_REPRESENTATION ( #9174, #16004 ) ;
#400 = CARTESIAN_POINT ( 'NONE',  ( -0.1765068388402301069, -5.153177966101685215, 7.347961541693647902 ) ) ;
#401 = EDGE_LOOP ( 'NONE', ( #12811, #11538, #1032, #13983, #10617, #10576, #15723, #6538 ) ) ;
#402 = DIRECTION ( 'NONE',  ( 0.000000000000000000, -1.000000000000000000, -1.332267629550190018E-15 ) ) ;
#403 = CARTESIAN_POINT ( 'NONE',  ( -1.925796468768790071, -0.4957627118644070130, 6.052706598917719560 ) ) ;
#404 = VERTEX_POINT ( 'NONE', #1430 ) ;
#405 = FACE_OUTER_BOUND ( 'NONE', #8642, .T. ) ;
#406 = DIRECTION ( 'NONE',  ( 1.142385477618690076E-14, -1.110223024625153952E-16, 1.000000000000000000 ) ) ;
#407 = CARTESIAN_POINT ( 'NONE',  ( 0.2047443300700049207, -2.192584066324520187, 2.657212296411530783 ) ) ;
#408 = CARTESIAN_POINT ( 'NONE',  ( 1.750000000000000000, 0.5999999999999999778, 7.700000000000000178 ) ) ;
#409 = CARTESIAN_POINT ( 'NONE',  ( 1.192209327851080136, -0.02224576271186471527, 2.329031440774910422 ) ) ;
#410 = VERTEX_POINT ( 'NONE', #11050 ) ;
#411 = DIRECTION ( 'NONE',  ( 2.220446049250309876E-16, 1.000000000000000000, -1.850371707708599740E-16 ) ) ;
#412 = VERTEX_POINT ( 'NONE', #2819 ) ;
#413 = CARTESIAN_POINT ( 'NONE',  ( 0.007090208766915150063, -0.3376261948321719886, 2.248104425785740101 ) ) ;
#414 = CARTESIAN_POINT ( 'NONE',  ( -0.3265524029357583236, -5.457627118644064801, 6.726831181542982208 ) ) ;
#415 = ADVANCED_FACE ( 'NONE', ( #12730 ), #3243, .T. ) ;
#416 = CARTESIAN_POINT ( 'NONE',  ( -1.000000000000000000, -7.000000000000000000, 5.700000000000000178 ) ) ;
#417 = EDGE_CURVE ( 'NONE', #7791, #16660, #1347, .T. ) ;
#418 = CARTESIAN_POINT ( 'NONE',  ( -1.873832970144350130, -0.2625000000000002331, 2.826167029855650270 ) ) ;
#419 = CARTESIAN_POINT ( 'NONE',  ( -2.589141052314440916, -3.287133615874059611, 5.282633936723525991 ) ) ;
#420 = ORIENTED_EDGE ( 'NONE', *, *, #10961, .F. ) ;
#421 = CARTESIAN_POINT ( 'NONE',  ( -1.167621112247339887, -2.778632149891699932, 6.743381174846780013 ) ) ;
#422 = DIRECTION ( 'NONE',  ( 0.000000000000000000, 0.000000000000000000, 1.000000000000000000 ) ) ;
#423 = PLANE ( 'NONE',  #3044 ) ;
#424 = CARTESIAN_POINT ( 'NONE',  ( -0.3429245540020551819, -1.823812330071880705, 2.675820019639910452 ) ) ;
#425 = PLANE ( 'NONE',  #7325 ) ;
#426 = ORIENTED_EDGE ( 'NONE', *, *, #18287, .T. ) ;
#427 = DIRECTION ( 'NONE',  ( -1.000000000000000000, 0.000000000000000000, 6.123233995736759873E-17 ) ) ;
#428 = CARTESIAN_POINT ( 'NONE',  ( -0.009452110982655128821, -0.5998079552954630467, 2.350000000000000089 ) ) ;
#429 = CARTESIAN_POINT ( 'NONE',  ( -2.549960444629829848, -1.544352870612421880, 3.964598460822165382 ) ) ;
#430 = VECTOR ( 'NONE', #9262, 1000.000000000000000 ) ;
#431 = FACE_OUTER_BOUND ( 'NONE', #10323, .T. ) ;
#432 = DIRECTION ( 'NONE',  ( -1.000000000000000000, 1.850371707708589879E-16, 7.401486830834380223E-16 ) ) ;
#433 = CARTESIAN_POINT ( 'NONE',  ( 0.6207106781186549904, 3.050000000000000266, 2.628553390593269423 ) ) ;
#434 = CARTESIAN_POINT ( 'NONE',  ( 2.328217775191430139, -5.081991525423729783, 5.043379051721160522 ) ) ;
#435 = VERTEX_POINT ( 'NONE', #9942 ) ;
#436 = EDGE_CURVE ( 'NONE', #3716, #6119, #18067, .T. ) ;
#437 = ORIENTED_EDGE ( 'NONE', *, *, #18165, .T. ) ;
#438 = CARTESIAN_POINT ( 'NONE',  ( 1.000000000000000000, -8.000000000000000000, 3.700000000000000178 ) ) ;
#439 = ADVANCED_FACE ( 'NONE', ( #5496 ), #3228, .T. ) ;
#440 = DIRECTION ( 'NONE',  ( 2.018587317500279868E-16, -1.000000000000000000, -1.009293658750139934E-16 ) ) ;
#441 = ORIENTED_EDGE ( 'NONE', *, *, #14504, .T. ) ;
#442 = CARTESIAN_POINT ( 'NONE',  ( 2.339254516529669647, -2.681638120378568857, 5.953396186326336270 ) ) ;
#443 = CARTESIAN_POINT ( 'NONE',  ( -1.750000000000000000, 0.5999999999999999778, 7.700000000000000178 ) ) ;
#444 = CARTESIAN_POINT ( 'NONE',  ( -0.5372984490435469551, 4.599999999999999645, 7.700000000000000178 ) ) ;
#445 = CARTESIAN_POINT ( 'NONE',  ( -0.3949552299395130417, -1.823812330071880039, 2.379923265530350385 ) ) ;
#446 = CARTESIAN_POINT ( 'NONE',  ( 1.487835687536851470, -5.028306595106930565, 2.490167689244129789 ) ) ;
#447 = CARTESIAN_POINT ( 'NONE',  ( -2.653777292528150866, -1.773394877135329839, 4.724078510415215426 ) ) ;
#448 = CARTESIAN_POINT ( 'NONE',  ( -1.850000000000000089, -6.000000000000000000, 2.299999999999999822 ) ) ;
#449 = CARTESIAN_POINT ( 'NONE',  ( -1.772995665808888788, -4.777584066324515710, 5.735078843205186239 ) ) ;
#450 = VECTOR ( 'NONE', #504, 1000.000000000000000 ) ;
#451 = DIRECTION ( 'NONE',  ( -0.2721173643531200059, -0.9622640697945191723, 0.000000000000000000 ) ) ;
#452 = ORIENTED_EDGE ( 'NONE', *, *, #9830, .T. ) ;
#453 = ADVANCED_FACE ( 'NONE', ( #10743 ), #5286, .T. ) ;
#454 = CARTESIAN_POINT ( 'NONE',  ( -0.009452110982656868748, -5.299807955295460005, 2.350000000000000089 ) ) ;
#455 = ORIENTED_EDGE ( 'NONE', *, *, #14444, .F. ) ;
#456 = CARTESIAN_POINT ( 'NONE',  ( -1.699999999999999956, 9.299999999999998934, 7.599999999999999645 ) ) ;
#457 = FACE_BOUND ( 'NONE', #15789, .T. ) ;
#458 = VERTEX_POINT ( 'NONE', #936 ) ;
#459 = CARTESIAN_POINT ( 'NONE',  ( 2.347833536521260367, -2.541908390648839777, 4.537447324629859224 ) ) ;
#460 = SURFACE_SIDE_STYLE ('',( #6019 ) ) ;
#461 = CARTESIAN_POINT ( 'NONE',  ( 1.811729841638690219, -5.341949152542369461, 3.197954009834290012 ) ) ;
#462 = CARTESIAN_POINT ( 'NONE',  ( 1.750000000000000000, 11.40000000000000036, 7.599999999999999645 ) ) ;
#463 = ADVANCED_FACE ( 'NONE', ( #6664 ), #1664, .T. ) ;
#464 = CARTESIAN_POINT ( 'NONE',  ( 2.287919158821199783, -1.051457940198389895, 5.251517552016890633 ) ) ;
#465 = CARTESIAN_POINT ( 'NONE',  ( 2.353452300571019506, -4.125511994252439862, 4.697179287168359529 ) ) ;
#466 = CARTESIAN_POINT ( 'NONE',  ( 1.688800633088581860, -0.8418633456037974971, 3.532586505616389871 ) ) ;
#467 =( REPRESENTATION_RELATIONSHIP ('NONE','NONE', #2757, #8322 ) REPRESENTATION_RELATIONSHIP_WITH_TRANSFORMATION ( #10465 )SHAPE_REPRESENTATION_RELATIONSHIP( ) );
#468 = DIRECTION ( 'NONE',  ( 6.123233995736769734E-17, 9.462128050782581713E-15, 1.000000000000000000 ) ) ;
#469 = VECTOR ( 'NONE', #13422, 1000.000000000000000 ) ;
#470 = DIRECTION ( 'NONE',  ( -6.123233995736769734E-17, -0.000000000000000000, -1.000000000000000000 ) ) ;
#471 = ORIENTED_EDGE ( 'NONE', *, *, #11105, .F. ) ;
#472 = ADVANCED_FACE ( 'NONE', ( #11019 ), #9341, .T. ) ;
#473 = CARTESIAN_POINT ( 'NONE',  ( 0.3803919826356921829, -0.3088983050847459166, 2.682580100125298461 ) ) ;
#474 = CARTESIAN_POINT ( 'NONE',  ( 0.4005155088302400634, -4.474836318576759453, 7.019123328904770531 ) ) ;
#475 = VERTEX_POINT ( 'NONE', #15390 ) ;
#476 = ORIENTED_EDGE ( 'NONE', *, *, #2348, .F. ) ;
#477 = DIRECTION ( 'NONE',  ( 0.000000000000000000, 0.000000000000000000, -1.000000000000000000 ) ) ;
#478 = ORIENTED_EDGE ( 'NONE', *, *, #1154, .F. ) ;
#479 = CARTESIAN_POINT ( 'NONE',  ( -0.2818998297622349325, -4.245794312053861042, 7.036509827384406890 ) ) ;
#480 = CARTESIAN_POINT ( 'NONE',  ( 1.031876288691629506, -5.130932203389829915, 7.145012538880298081 ) ) ;
#481 = CLOSED_SHELL ( 'NONE', ( #1105, #2707, #9593, #6776, #453, #11667, #7385, #17067, #8138, #15405, #12267, #12757, #9929, #9494, #12651, #4830, #16140, #8466, #10660, #15825, #4528, #1215, #9827, #12773, #4933, #13085, #185, #8268, #11635, #10825, #9835, #17731, #4480, #14796, #4935, #10301, #12187, #10144, #17825, #8156, #17296, #10851, #7547, #10060, #2024, #10760, #7033, #12336, #16058, #1303, #16617, #2049, #15657, #8174, #18268, #10717, #6978, #4586, #7790, #17935, #10266, #3976, #14973, #16625, #13703, #9469, #12597, #1004, #8913, #17259, #1134, #13104, #11381, #542, #2399, #8141, #3638, #14784, #10475, #11632, #17413, #6182, #5439, #4021, #637, #11519, #640, #13095, #2808, #6975, #5978, #17597, #9926, #7014, #12152, #17426, #2903, #9854, #17163, #928, #2476, #15539, #9487, #1231, #11443, #10206, #8402, #9245, #8488, #12540, #15092, #17970, #9951, #905, #10315, #7709, #12982, #2010, #8698, #15268, #13903, #15387, #5590, #1452, #4154, #7892, #3027, #13438, #2170, #8041, #6286, #15148, #12120, #173, #4067, #18029, #7347, #6752, #6683, #5308, #14678, #12014, #16384, #16822, #2892, #6701 ) ) ;
#482 = AXIS2_PLACEMENT_3D ( 'NONE', #15870, #14482, #11517 ) ;
#483 = LINE ( 'NONE', #664, #7613 ) ;
#484 = CARTESIAN_POINT ( 'NONE',  ( -2.293398556041709835, -0.5358050847457630494, 4.171956209133480975 ) ) ;
#485 = ORIENTED_EDGE ( 'NONE', *, *, #13436, .T. ) ;
#486 = CARTESIAN_POINT ( 'NONE',  ( -1.899999999999999911, 11.15000000000000036, 7.990820364436479856E-16 ) ) ;
#487 = CARTESIAN_POINT ( 'NONE',  ( 1.889999999999999902, 4.100000000000000533, -6.512531667206379696E-16 ) ) ;
#488 = CARTESIAN_POINT ( 'NONE',  ( -1.937109463115380903, -3.426863345603793576, 4.019920026366796684 ) ) ;
#489 = CARTESIAN_POINT ( 'NONE',  ( -1.666450993087168930, -0.4824152542372879826, 6.765380371283871597 ) ) ;
#490 = VERTEX_POINT ( 'NONE', #3889 ) ;
#491 = LINE ( 'NONE', #17068, #7903 ) ;
#492 = CIRCLE ( 'NONE', #4337, 0.5999999999999998668 ) ;
#493 = EDGE_LOOP ( 'NONE', ( #3979, #4841, #1424, #2607 ) ) ;
#494 = CARTESIAN_POINT ( 'NONE',  ( -0.009227126607029439292, -0.5962421434521730790, 2.310024366371980165 ) ) ;
#495 = CARTESIAN_POINT ( 'NONE',  ( 0.06264882350516240428, -5.448728813559320372, 7.052569299041220319 ) ) ;
#496 = CARTESIAN_POINT ( 'NONE',  ( -1.811729841638699767, -0.2580508474576270195, 3.197954009834300226 ) ) ;
#497 = VECTOR ( 'NONE', #10509, 1000.000000000000000 ) ;
#498 = CARTESIAN_POINT ( 'NONE',  ( 1.155768864438629695, -4.404971453711897134, 7.088998121597438029 ) ) ;
#499 = ORIENTED_EDGE ( 'NONE', *, *, #14133, .T. ) ;
#500 = CARTESIAN_POINT ( 'NONE',  ( 2.334032080503399609, -2.289578095837639715, 5.001728246382190157 ) ) ;
#501 = AXIS2_PLACEMENT_3D ( 'NONE', #17888, #13465, #603 ) ;
#502 = CARTESIAN_POINT ( 'NONE',  ( 1.899999999999999911, 9.199999999999999289, 0.6099999999999999867 ) ) ;
#503 = AXIS2_PLACEMENT_3D ( 'NONE', #7453, #4395, #3187 ) ;
#504 = DIRECTION ( 'NONE',  ( 5.551115123125779621E-17, 0.000000000000000000, 1.000000000000000000 ) ) ;
#505 = CARTESIAN_POINT ( 'NONE',  ( 0.7368491673939637776, -3.523857375116919322, 2.783765372628159263 ) ) ;
#506 = DIRECTION ( 'NONE',  ( 1.000000000000000000, 1.283953296258166085E-32, -6.123233995736769734E-17 ) ) ;
#507 = CARTESIAN_POINT ( 'NONE',  ( -0.3750000000000000000, 3.050000000000000266, 2.100000000000000089 ) ) ;
#508 = CARTESIAN_POINT ( 'NONE',  ( 0.4114611322411816374, -1.032010528270079330, 6.711368086473216366 ) ) ;
#509 = ORIENTED_EDGE ( 'NONE', *, *, #12081, .T. ) ;
#510 = EDGE_CURVE ( 'NONE', #2436, #16660, #16741, .T. ) ;
#511 = AXIS2_PLACEMENT_3D ( 'NONE', #3068, #18227, #15681 ) ;
#512 = CARTESIAN_POINT ( 'NONE',  ( 1.800000000000000044, 11.40000000000000036, 1.600000000000000089 ) ) ;
#513 = CIRCLE ( 'NONE', #1410, 0.2500000000000002220 ) ;
#514 = VECTOR ( 'NONE', #10308, 1000.000000000000000 ) ;
#515 = DIRECTION ( 'NONE',  ( 1.059337802663170094E-14, 1.000000000000000000, 1.929541063032960169E-30 ) ) ;
#516 = CARTESIAN_POINT ( 'NONE',  ( 0.7756407636289058827, -1.008722239981790558, 7.238010066725317770 ) ) ;
#517 = EDGE_LOOP ( 'NONE', ( #11060, #3583, #4007, #16442 ) ) ;
#518 = DIRECTION ( 'NONE',  ( -2.337311630789800155E-16, 1.000000000000000000, 0.000000000000000000 ) ) ;
#519 = DIRECTION ( 'NONE',  ( 1.000000000000000000, -1.103950578158349959E-14, 0.000000000000000000 ) ) ;
#520 = CARTESIAN_POINT ( 'NONE',  ( 1.550000000000000044, -6.000000000000000000, 5.100000000000000533 ) ) ;
#521 = CARTESIAN_POINT ( 'NONE',  ( 1.477796163681079911, -5.117584745762710163, 6.531563725478140015 ) ) ;
#522 = ORIENTED_EDGE ( 'NONE', *, *, #6504, .F. ) ;
#523 = VECTOR ( 'NONE', #3659, 1000.000000000000000 ) ;
#524 = ORIENTED_EDGE ( 'NONE', *, *, #10146, .F. ) ;
#525 = CARTESIAN_POINT ( 'NONE',  ( 2.500000000000000000, 10.00000000000000000, -5.075305255429290705E-16 ) ) ;
#526 = DIRECTION ( 'NONE',  ( -2.220446049250309876E-16, -1.000000000000000000, 4.930380657631319405E-32 ) ) ;
#527 = ORIENTED_EDGE ( 'NONE', *, *, #3623, .T. ) ;
#528 = EDGE_CURVE ( 'NONE', #17501, #10555, #13235, .T. ) ;
#529 = AXIS2_PLACEMENT_3D ( 'NONE', #9899, #3969, #6850 ) ;
#530 = CARTESIAN_POINT ( 'NONE',  ( -0.1110902655589390137, -2.961097579838030569, 7.351560417169478612 ) ) ;
#531 = VECTOR ( 'NONE', #12503, 1000.000000000000000 ) ;
#532 = ADVANCED_FACE ( 'NONE', ( #12413 ), #10936, .F. ) ;
#533 = LINE ( 'NONE', #14427, #12662 ) ;
#534 = CARTESIAN_POINT ( 'NONE',  ( 2.500000000000000000, 9.199999999999999289, 1.600000000000000089 ) ) ;
#535 = CARTESIAN_POINT ( 'NONE',  ( 2.036228139452630259, -2.126560077819629857, 3.519948877554369915 ) ) ;
#536 = EDGE_CURVE ( 'NONE', #3882, #3854, #4603, .T. ) ;
#537 = CARTESIAN_POINT ( 'NONE',  ( -0.1749999999999999889, 8.200000000000001066, 0.4000000000000000222 ) ) ;
#538 = AXIS2_PLACEMENT_3D ( 'NONE', #1149, #15052, #18243 ) ;
#539 = CARTESIAN_POINT ( 'NONE',  ( -2.161802606005209793, -5.010466949207389220, 3.769755311421840283 ) ) ;
#540 = EDGE_CURVE ( 'NONE', #10260, #6008, #5380, .T. ) ;
#541 = CARTESIAN_POINT ( 'NONE',  ( 1.399999999999999911, -5.500000000000000000, 5.100000000000000533 ) ) ;
#542 = ADVANCED_FACE ( 'NONE', ( #18116 ), #8251, .F. ) ;
#543 = VECTOR ( 'NONE', #1826, 1000.000000000000000 ) ;
#544 = VECTOR ( 'NONE', #5083, 1000.000000000000000 ) ;
#545 = DIRECTION ( 'NONE',  ( -4.440892098500630106E-16, 0.000000000000000000, 1.000000000000000000 ) ) ;
#546 = EDGE_LOOP ( 'NONE', ( #14496, #12522, #5384, #16838 ) ) ;
#547 = VECTOR ( 'NONE', #6134, 1000.000000000000000 ) ;
#548 = FACE_OUTER_BOUND ( 'NONE', #2723, .T. ) ;
#549 = ORIENTED_EDGE ( 'NONE', *, *, #17371, .T. ) ;
#550 = DIRECTION ( 'NONE',  ( -1.000000000000000000, -8.881784197001249119E-17, -1.776356839400249824E-16 ) ) ;
#551 = DIRECTION ( 'NONE',  ( 0.000000000000000000, -1.000000000000000000, 0.000000000000000000 ) ) ;
#552 =( GEOMETRIC_REPRESENTATION_CONTEXT ( 3 ) GLOBAL_UNCERTAINTY_ASSIGNED_CONTEXT ( ( #2517 ) ) GLOBAL_UNIT_ASSIGNED_CONTEXT ( ( #4504, #3040, #6174 ) ) REPRESENTATION_CONTEXT ( 'NONE', 'WORKASPACE' ) );
#553 = ORIENTED_EDGE ( 'NONE', *, *, #10570, .F. ) ;
#554 = DIRECTION ( 'NONE',  ( 1.306144734853129823E-16, -1.000000000000000000, -6.530723674265629391E-17 ) ) ;
#555 = CARTESIAN_POINT ( 'NONE',  ( 0.4539185741479240255, -2.215872354612800521, 2.390735265170440105 ) ) ;
#556 = EDGE_CURVE ( 'NONE', #14368, #9144, #15286, .T. ) ;
#557 = SPHERICAL_SURFACE ( 'NONE', #241, 0.8000000000000000444 ) ;
#558 = CARTESIAN_POINT ( 'NONE',  ( -2.500000000000000000, 10.00000000000000000, 1.600000000000000089 ) ) ;
#559 = VECTOR ( 'NONE', #7948, 1000.000000000000000 ) ;
#560 = FACE_BOUND ( 'NONE', #795, .T. ) ;
#561 = ADVANCED_FACE ( 'NONE', ( #4065 ), #6855, .F. ) ;
#562 = FACE_OUTER_BOUND ( 'NONE', #15, .T. ) ;
#563 = CARTESIAN_POINT ( 'NONE',  ( 0.4005155088302400634, -4.474836318576759453, 7.019123328904770531 ) ) ;
#564 = CARTESIAN_POINT ( 'NONE',  ( 2.050994839075679366, -0.9815930753335269099, 4.608774933727144862 ) ) ;
#565 = CARTESIAN_POINT ( 'NONE',  ( 0.8731223871105069367, -0.1290254237288140371, 6.558046933601105799 ) ) ;
#566 = CARTESIAN_POINT ( 'NONE',  ( 2.500000000000000000, 4.700000000000000178, 1.600000000000000089 ) ) ;
#567 = DIRECTION ( 'NONE',  ( 0.000000000000000000, 0.000000000000000000, -1.000000000000000000 ) ) ;
#568 = ORIENTED_EDGE ( 'NONE', *, *, #93, .F. ) ;
#569 = CARTESIAN_POINT ( 'NONE',  ( -0.9707742057416274273, -0.1735169491525429541, 6.508944043303927174 ) ) ;
#570 = CARTESIAN_POINT ( 'NONE',  ( -2.351999299633229956, -3.333710192450639820, 4.782734406438290620 ) ) ;
#571 = ORIENTED_EDGE ( 'NONE', *, *, #11074, .T. ) ;
#572 = AXIS2_PLACEMENT_3D ( 'NONE', #3697, #17666, #14917 ) ;
#573 = ORIENTED_EDGE ( 'NONE', *, *, #11966, .T. ) ;
#574 = CARTESIAN_POINT ( 'NONE',  ( 2.616666666666669805, -6.661338147750939243E-16, 7.649999999999999467 ) ) ;
#575 = ORIENTED_EDGE ( 'NONE', *, *, #10898, .F. ) ;
#576 = FACE_OUTER_BOUND ( 'NONE', #11007, .T. ) ;
#577 = ITEM_DEFINED_TRANSFORMATION ( 'NONE', 'NONE', #8257,  #17681 ) ;
#578 = CARTESIAN_POINT ( 'NONE',  ( -1.610878918935079840, -5.568855932203385706, 2.590989782159090815 ) ) ;
#579 = DIRECTION ( 'NONE',  ( 1.000000000000000000, 0.000000000000000000, 0.000000000000000000 ) ) ;
#580 = CARTESIAN_POINT ( 'NONE',  ( 2.306642602145299925, -0.3845338983050849979, 5.166805192608480368 ) ) ;
#581 = ORIENTED_EDGE ( 'NONE', *, *, #8066, .F. ) ;
#582 = EDGE_CURVE ( 'NONE', #14617, #14203, #6481, .T. ) ;
#583 = DIRECTION ( 'NONE',  ( 0.000000000000000000, 1.000000000000000000, 0.000000000000000000 ) ) ;
#584 = FACE_BOUND ( 'NONE', #16591, .T. ) ;
#585 = VECTOR ( 'NONE', #11479, 1000.000000000000000 ) ;
#586 = CARTESIAN_POINT ( 'NONE',  ( 1.974086094277279768, -4.195376859117311064, 5.263813741415705572 ) ) ;
#587 = CARTESIAN_POINT ( 'NONE',  ( 1.554165089654128584, -0.1201271186440679706, 6.851145244874527584 ) ) ;
#588 = ORIENTED_EDGE ( 'NONE', *, *, #1576, .T. ) ;
#589 = ORIENTED_EDGE ( 'NONE', *, *, #4710, .F. ) ;
#590 = CARTESIAN_POINT ( 'NONE',  ( -2.431060148753501515, -0.5447033898305090327, 3.635668498923334102 ) ) ;
#591 = ORIENTED_EDGE ( 'NONE', *, *, #1780, .F. ) ;
#592 = CARTESIAN_POINT ( 'NONE',  ( 1.828929293328490072E-16, 2.399999999999999911, 5.100000000000000533 ) ) ;
#593 = CARTESIAN_POINT ( 'NONE',  ( -1.800000000000000044, 12.00000000000000000, 1.600000000000000089 ) ) ;
#594 = DIRECTION ( 'NONE',  ( -6.476300976980080477E-16, 9.251858538542978977E-17, -1.000000000000000000 ) ) ;
#595 = AXIS2_PLACEMENT_3D ( 'NONE', #12279, #13477, #898 ) ;
#596 = CARTESIAN_POINT ( 'NONE',  ( 2.642175029090480631, -4.102223705964154199, 4.450952196049445142 ) ) ;
#597 = ORIENTED_EDGE ( 'NONE', *, *, #12740, .F. ) ;
#598 = ADVANCED_FACE ( 'NONE', ( #11204 ), #1488, .T. ) ;
#599 = CARTESIAN_POINT ( 'NONE',  ( 2.295719155670170153, -2.312866384125930264, 5.218091927917190453 ) ) ;
#600 = CARTESIAN_POINT ( 'NONE',  ( 2.500000000000000000, 11.25000000000000000, 7.649999999999999467 ) ) ;
#601 = CARTESIAN_POINT ( 'NONE',  ( 5.829811056852189859E-17, 3.957026083511942627, 8.102080397533576672 ) ) ;
#602 = CARTESIAN_POINT ( 'NONE',  ( 0.6965028529799376367, -4.129352870612409632, 6.631265289497767057 ) ) ;
#603 = DIRECTION ( 'NONE',  ( 1.836970198721028208E-16, -6.938893903907222067E-15, 1.000000000000000000 ) ) ;
#604 = CARTESIAN_POINT ( 'NONE',  ( 1.673492459604400961, -2.103271789531340641, 3.510746103527379702 ) ) ;
#605 = ORIENTED_EDGE ( 'NONE', *, *, #12076, .T. ) ;
#606 = CIRCLE ( 'NONE', #11850, 0.1999999999999999833 ) ;
#607 = LINE ( 'NONE', #6245, #10557 ) ;
#608 = CARTESIAN_POINT ( 'NONE',  ( 0.8469861386668179337, -0.7068739681193977331, 2.826929786773349385 ) ) ;
#609 = CARTESIAN_POINT ( 'NONE',  ( 1.648422021521518621, -0.9155690868286361361, 6.779860219333207816 ) ) ;
#610 = EDGE_LOOP ( 'NONE', ( #17972, #13262, #16216, #12238 ) ) ;
#611 = CARTESIAN_POINT ( 'NONE',  ( 2.353452300571019506, -4.125511994252439862, 4.697179287168359529 ) ) ;
#612 = CARTESIAN_POINT ( 'NONE',  ( -3.992840858131154872E-17, 4.942973916488066166, 6.497919602466422084 ) ) ;
#613 = DIRECTION ( 'NONE',  ( 0.000000000000000000, 1.000000000000000000, 0.000000000000000000 ) ) ;
#614 = CARTESIAN_POINT ( 'NONE',  ( -1.978267656359410154, -5.197669491525420682, 5.974740860598790171 ) ) ;
#615 = ORIENTED_EDGE ( 'NONE', *, *, #5753, .F. ) ;
#616 = VERTEX_POINT ( 'NONE', #16849 ) ;
#617 = CARTESIAN_POINT ( 'NONE',  ( 2.500000000000000000, 4.700000000000000178, 0.5999999999999999778 ) ) ;
#618 = PLANE ( 'NONE',  #12952 ) ;
#619 = LINE ( 'NONE', #17535, #497 ) ;
#620 = VERTEX_POINT ( 'NONE', #1657 ) ;
#621 = PLANE ( 'NONE',  #16828 ) ;
#622 = CARTESIAN_POINT ( 'NONE',  ( 0.7540633504677742849, -2.239160642901089293, 2.155495695330191364 ) ) ;
#623 = DIRECTION ( 'NONE',  ( 1.000000000000000000, -2.220446049250309876E-16, 0.000000000000000000 ) ) ;
#624 = DIRECTION ( 'NONE',  ( 1.000000000000000000, 0.000000000000000000, 0.000000000000000000 ) ) ;
#625 = CARTESIAN_POINT ( 'NONE',  ( -0.6673090596498669758, -3.360839357098900138, 2.443133963569589895 ) ) ;
#626 = CARTESIAN_POINT ( 'NONE',  ( 0.2435295127647320035, -5.004947479095229745, 2.350795284704489507 ) ) ;
#627 = CARTESIAN_POINT ( 'NONE',  ( -2.543624461644929724, -1.703530012270459970, 5.457025951420040322 ) ) ;
#628 = CARTESIAN_POINT ( 'NONE',  ( -1.850000000000000089, 0.7500000000000000000, 7.700000000000000178 ) ) ;
#629 = CARTESIAN_POINT ( 'NONE',  ( 1.110223024625159893E-15, 0.3264109415988649676, 5.199061676633699669 ) ) ;
#630 = CARTESIAN_POINT ( 'NONE',  ( -2.500000000000000000, 10.00000000000000000, 1.600000000000000089 ) ) ;
#631 = CARTESIAN_POINT ( 'NONE',  ( -2.353194804772640314, -5.524364406779660008, 4.731327187377240229 ) ) ;
#632 = ORIENTED_EDGE ( 'NONE', *, *, #4794, .T. ) ;
#633 = FACE_OUTER_BOUND ( 'NONE', #18025, .T. ) ;
#634 = EDGE_LOOP ( 'NONE', ( #3635, #12875, #12092, #13287 ) ) ;
#635 = CARTESIAN_POINT ( 'NONE',  ( -1.899999999999999911, 2.000000000000000000, 1.600000000000000089 ) ) ;
#636 = DIRECTION ( 'NONE',  ( 1.000000000000000000, 0.000000000000000000, 0.000000000000000000 ) ) ;
#637 = ADVANCED_FACE ( 'NONE', ( #1577 ), #1380, .F. ) ;
#638 = ORIENTED_EDGE ( 'NONE', *, *, #18114, .F. ) ;
#639 = EDGE_CURVE ( 'NONE', #9659, #10455, #8614, .T. ) ;
#640 = ADVANCED_FACE ( 'NONE', ( #9905 ), #12783, .F. ) ;
#641 = CARTESIAN_POINT ( 'NONE',  ( -0.5320716618283710675, -3.007674156414609890, 6.992519451207139802 ) ) ;
#642 = CARTESIAN_POINT ( 'NONE',  ( -1.899999999999999911, 2.000000000000000000, 1.600000000000000089 ) ) ;
#643 = CARTESIAN_POINT ( 'NONE',  ( 2.058670345754650022, -5.350847457627120107, 3.559656372813920111 ) ) ;
#644 = PLANE ( 'NONE',  #2134 ) ;
#645 = CARTESIAN_POINT ( 'NONE',  ( -2.091095264232510242, -1.656953435693890198, 5.779845490516250628 ) ) ;
#646 = CIRCLE ( 'NONE', #2745, 0.2999999999999999334 ) ;
#647 = CARTESIAN_POINT ( 'NONE',  ( 0.5133516189064986079, -4.152641158900696183, 6.687805814961351736 ) ) ;
#648 = B_SPLINE_CURVE_WITH_KNOTS ( 'NONE', 3,
 ( #13687, #15087, #10621, #17733, #16359, #12289, #10909 ),
 .UNSPECIFIED., .F., .F.,
 ( 4, 1, 1, 1, 4 ),
 ( 0.000000000000000000, 0.3003308066897660278, 0.4325493167368040237, 0.5576349185195599301, 0.7853981633974479459 ),
 .UNSPECIFIED. ) ;
#649 = DIRECTION ( 'NONE',  ( -1.000000000000000000, 0.000000000000000000, 1.586032892321649771E-16 ) ) ;
#650 = DIRECTION ( 'NONE',  ( 1.000000000000000000, 0.000000000000000000, 0.000000000000000000 ) ) ;
#651 = VERTEX_POINT ( 'NONE', #2782 ) ;
#652 = CARTESIAN_POINT ( 'NONE',  ( 1.608484968265039949, -0.5211538081685300750, 3.106608516387050045 ) ) ;
#653 = EDGE_CURVE ( 'NONE', #14665, #6595, #1073, .T. ) ;
#654 = CARTESIAN_POINT ( 'NONE',  ( -1.695509042132779864, -0.2536016949152540834, 3.542446458728619518 ) ) ;
#655 = CARTESIAN_POINT ( 'NONE',  ( 1.567709126316360058, -3.915917399657849796, 2.944712621036570166 ) ) ;
#656 = ORIENTED_EDGE ( 'NONE', *, *, #14817, .T. ) ;
#657 = ORIENTED_EDGE ( 'NONE', *, *, #1694, .T. ) ;
#658 = CARTESIAN_POINT ( 'NONE',  ( 0.6628679656440349399, 3.050000000000000266, 1.670710678118660031 ) ) ;
#659 = EDGE_CURVE ( 'NONE', #4099, #9483, #12309, .T. ) ;
#660 = ORIENTED_EDGE ( 'NONE', *, *, #4794, .F. ) ;
#661 = CARTESIAN_POINT ( 'NONE',  ( -2.350542563031990273, -4.595118636378179744, 4.817027120179790067 ) ) ;
#662 = EDGE_CURVE ( 'NONE', #12922, #16401, #2973, .T. ) ;
#663 = CARTESIAN_POINT ( 'NONE',  ( 2.234315482767910144, -5.059745762711860273, 3.960850823455320580 ) ) ;
#664 = CARTESIAN_POINT ( 'NONE',  ( 1.875000000000000000, 12.00000000000000000, 7.700000000000000178 ) ) ;
#665 = CARTESIAN_POINT ( 'NONE',  ( -2.328217775191430139, -0.5180084745762719711, 5.043379051721170292 ) ) ;
#666 = ORIENTED_EDGE ( 'NONE', *, *, #14756, .T. ) ;
#667 = AXIS2_PLACEMENT_3D ( 'NONE', #10886, #9774, #16898 ) ;
#668 = DIRECTION ( 'NONE',  ( 0.7071067811865466846, 0.000000000000000000, -0.7071067811865483499 ) ) ;
#669 = CARTESIAN_POINT ( 'NONE',  ( 0.3509990757148593321, -4.474836318576761229, 6.722795464567642654 ) ) ;
#670 = CARTESIAN_POINT ( 'NONE',  ( -2.304156201936080617, -0.5002118644067795605, 6.016707707703351282 ) ) ;
#671 = ORIENTED_EDGE ( 'NONE', *, *, #7463, .F. ) ;
#672 = CARTESIAN_POINT ( 'NONE',  ( 1.128670402850170174, -0.4290254237288141370, 7.101865548313628373 ) ) ;
#673 = EDGE_LOOP ( 'NONE', ( #2543, #4016, #8725, #4883 ) ) ;
#674 = CARTESIAN_POINT ( 'NONE',  ( -2.270487904532170198, -5.537711864406779760, 4.080813552109679776 ) ) ;
#675 = LINE ( 'NONE', #16416, #12071 ) ;
#676 = ADVANCED_FACE ( 'NONE', ( #14257 ), #8520, .T. ) ;
#677 = AXIS2_PLACEMENT_3D ( 'NONE', #7128, #8673, #12764 ) ;
#678 = LINE ( 'NONE', #7808, #7149 ) ;
#679 = CARTESIAN_POINT ( 'NONE',  ( 0.6890111762202997259, -3.799475958216412153, 2.137115435286760956 ) ) ;
#680 = ORIENTED_EDGE ( 'NONE', *, *, #8608, .T. ) ;
#681 = CARTESIAN_POINT ( 'NONE',  ( 2.237394498046680003, -2.336154672414219924, 5.429939413646329704 ) ) ;
#682 = EDGE_CURVE ( 'NONE', #13202, #15500, #5739, .T. ) ;
#683 = DIRECTION ( 'NONE',  ( 1.224646799147350002E-16, -1.000000000000000000, -6.123233995736769734E-17 ) ) ;
#684 = FACE_OUTER_BOUND ( 'NONE', #16904, .T. ) ;
#685 = CARTESIAN_POINT ( 'NONE',  ( -1.985741519624380835, -3.104668185927728974, 4.178720363079513334 ) ) ;
#686 = ADVANCED_BREP_SHAPE_REPRESENTATION ( '', ( #7724, #17681 ), #552 ) ;
#687 = LINE ( 'NONE', #17603, #4352 ) ;
#688 = DIRECTION ( 'NONE',  ( -1.000000000000000000, 1.224646799147350002E-16, 0.000000000000000000 ) ) ;
#689 = ADVANCED_FACE ( 'NONE', ( #2688 ), #9940, .T. ) ;
#690 = CARTESIAN_POINT ( 'NONE',  ( -0.1608173401625278554, -1.101875393134940984, 6.746714348835997299 ) ) ;
#691 = EDGE_LOOP ( 'NONE', ( #9977, #3355, #6508, #17403, #8904, #10550 ) ) ;
#692 = DIRECTION ( 'NONE',  ( 3.700743415417190112E-16, 1.000000000000000000, 0.000000000000000000 ) ) ;
#693 = FACE_BOUND ( 'NONE', #4148, .T. ) ;
#694 = CARTESIAN_POINT ( 'NONE',  ( -1.373536515609910191, -1.218316834576379737, 6.970795264502737787 ) ) ;
#695 = ORIENTED_EDGE ( 'NONE', *, *, #1552, .T. ) ;
#696 = PLANE ( 'NONE',  #836 ) ;
#697 = CARTESIAN_POINT ( 'NONE',  ( -2.500000000000000000, 2.000000000000000000, 1.600000000000000089 ) ) ;
#698 = DIRECTION ( 'NONE',  ( 1.000000000000000000, 0.000000000000000000, 2.865091676452019757E-16 ) ) ;
#699 = CARTESIAN_POINT ( 'NONE',  ( 1.695509042132770761, -5.046398305084744962, 3.542446458728613301 ) ) ;
#700 = ORIENTED_EDGE ( 'NONE', *, *, #7126, .T. ) ;
#701 = EDGE_CURVE ( 'NONE', #5888, #1832, #17295, .T. ) ;
#702 = ORIENTED_EDGE ( 'NONE', *, *, #16197, .T. ) ;
#703 = LINE ( 'NONE', #12194, #7706 ) ;
#704 = DIRECTION ( 'NONE',  ( 0.000000000000000000, -1.000000000000000000, 0.000000000000000000 ) ) ;
#705 = CARTESIAN_POINT ( 'NONE',  ( -0.009452110982655708218, -0.5998079552954630467, 2.350000000000000089 ) ) ;
#706 = ORIENTED_EDGE ( 'NONE', *, *, #14653, .F. ) ;
#707 = CARTESIAN_POINT ( 'NONE',  ( -2.052786957354850728, -5.524364406779660897, 4.727327971967373976 ) ) ;
#708 = CARTESIAN_POINT ( 'NONE',  ( 2.652303127816839190, -2.266289807549351387, 4.791661394135748431 ) ) ;
#709 = CARTESIAN_POINT ( 'NONE',  ( -1.800000000000000044, 11.40000000000000036, 7.649999999999999467 ) ) ;
#710 = CARTESIAN_POINT ( 'NONE',  ( 0.3832714063289482387, -2.914521003261450360, 7.326064873930673294 ) ) ;
#711 = EDGE_CURVE ( 'NONE', #12486, #8493, #10165, .T. ) ;
#712 = DIRECTION ( 'NONE',  ( 0.000000000000000000, 0.000000000000000000, 1.000000000000000000 ) ) ;
#713 = CARTESIAN_POINT ( 'NONE',  ( 0.5000000000000000000, 4.631370849898480024, 6.100000000000000533 ) ) ;
#714 = CARTESIAN_POINT ( 'NONE',  ( 0.8001898266890951072, -4.129352870612410520, 6.913242401714550844 ) ) ;
#715 = FACE_OUTER_BOUND ( 'NONE', #5104, .T. ) ;
#716 = CARTESIAN_POINT ( 'NONE',  ( 0.1749999999999999889, 9.199999999999999289, 0.4000000000000000222 ) ) ;
#718 = EDGE_LOOP ( 'NONE', ( #2340, #1566, #11515, #12930 ) ) ;
#717 = CARTESIAN_POINT ( 'NONE',  ( 0.02098813186351079427, -2.169295778036230526, 2.046196467083000403 ) ) ;
#719 = DIRECTION ( 'NONE',  ( 1.000000000000000000, -1.224646799147350002E-16, 0.000000000000000000 ) ) ;
#720 = CARTESIAN_POINT ( 'NONE',  ( -1.399999999999999911, -9.500000000000000000, 3.299999999999999822 ) ) ;
#721 = CARTESIAN_POINT ( 'NONE',  ( -2.316639661709700260, -1.819971453711900056, 4.285359956977770501 ) ) ;
#722 = DIRECTION ( 'NONE',  ( 2.114710523095539848E-16, 1.000000000000000000, -8.458842092382139670E-17 ) ) ;
#723 = CARTESIAN_POINT ( 'NONE',  ( -1.000896394980330006, -5.470974576271190770, 6.829956240957379521 ) ) ;
#724 = ORIENTED_EDGE ( 'NONE', *, *, #11762, .T. ) ;
#725 = DIRECTION ( 'NONE',  ( -1.000000000000000000, 0.000000000000000000, 1.224646799147350002E-16 ) ) ;
#726 = ORIENTED_EDGE ( 'NONE', *, *, #13, .T. ) ;
#727 = CARTESIAN_POINT ( 'NONE',  ( -0.8740908734716290596, 4.154758922476410099, 7.700000000000000178 ) ) ;
#728 = LINE ( 'NONE', #6194, #11194 ) ;
#729 = EDGE_LOOP ( 'NONE', ( #8849, #12695, #15570, #11829, #11114, #5194 ) ) ;
#730 = ORIENTED_EDGE ( 'NONE', *, *, #9132, .F. ) ;
#731 = ADVANCED_FACE ( 'NONE', ( #17191 ), #1295, .F. ) ;
#732 = CARTESIAN_POINT ( 'NONE',  ( 1.962536940652990003, -2.704926408666860294, 5.998920491814760503 ) ) ;
#733 =( BOUNDED_SURFACE ( )  B_SPLINE_SURFACE ( 3, 3, ( 
 ( #4152, #5646, #9810, #11289, #18030, #15467, #5376 ),
 ( #8513, #2776, #11014, #12683, #14163, #16663, #5817 ),
 ( #14519, #5913, #170, #10428, #1838, #1752, #17103 ),
 ( #14601, #14332, #3045, #15913, #11734, #10345, #7399 ),
 ( #13038, #13131, #11836, #14251, #13212, #1569, #8685 ),
 ( #5998, #1652, #16091, #8607, #360, #4427, #7214 ),
 ( #274, #3122, #4778, #1916, #10087, #8870, #7299 ) ),
 .UNSPECIFIED., .T., .F., .F. ) 
 B_SPLINE_SURFACE_WITH_KNOTS ( ( 4, 3, 4 ),
 ( 4, 1, 1, 1, 4 ),
 ( 0.000000000000000000, 3.141592653589790007, 6.283185307179590673 ),
 ( 0.000000000000000000, 0.3003308066897660278, 0.4325493167368040237, 0.5576349185195599301, 0.7853981633974479459 ),
 .UNSPECIFIED. ) 
 GEOMETRIC_REPRESENTATION_ITEM ( )  RATIONAL_B_SPLINE_SURFACE ( (
 ( 1.000000000000000000, 1.000000000000000000, 1.000000000000000000, 1.000000000000000000, 1.000000000000000000, 1.000000000000000000, 1.000000000000000000),
 ( 0.3333333333333329818, 0.3333333333333329818, 0.3333333333333329818, 0.3333333333333329818, 0.3333333333333329818, 0.3333333333333329818, 0.3333333333333329818),
 ( 0.3333333333333329818, 0.3333333333333329818, 0.3333333333333329818, 0.3333333333333329818, 0.3333333333333329818, 0.3333333333333329818, 0.3333333333333329818),
 ( 1.000000000000000000, 1.000000000000000000, 1.000000000000000000, 1.000000000000000000, 1.000000000000000000, 1.000000000000000000, 1.000000000000000000),
 ( 0.3333333333333329818, 0.3333333333333329818, 0.3333333333333329818, 0.3333333333333329818, 0.3333333333333329818, 0.3333333333333329818, 0.3333333333333329818),
 ( 0.3333333333333329818, 0.3333333333333329818, 0.3333333333333329818, 0.3333333333333329818, 0.3333333333333329818, 0.3333333333333329818, 0.3333333333333329818),
 ( 1.000000000000000000, 1.000000000000000000, 1.000000000000000000, 1.000000000000000000, 1.000000000000000000, 1.000000000000000000, 1.000000000000000000) ) ) 
 REPRESENTATION_ITEM ( '' )  SURFACE ( )  );
#734 = DIRECTION ( 'NONE',  ( 1.000000000000000000, 0.000000000000000000, 0.000000000000000000 ) ) ;
#735 = CARTESIAN_POINT ( 'NONE',  ( -1.707817112497179934, -5.488771186440679628, 6.319218296629480314 ) ) ;
#736 = PLANE ( 'NONE',  #17898 ) ;
#737 = CARTESIAN_POINT ( 'NONE',  ( 2.347833536521260367, -2.541908390648839777, 4.537447324629859224 ) ) ;
#738 = CARTESIAN_POINT ( 'NONE',  ( 1.219286470748990103, -4.381683165423610582, 6.712979431025659416 ) ) ;
#739 = CARTESIAN_POINT ( 'NONE',  ( 0.6217226704572607066, -1.307629111369559949, 6.656620240022977697 ) ) ;
#740 = CARTESIAN_POINT ( 'NONE',  ( -1.800000000000000044, 0.5999999999999999778, 1.600000000000000089 ) ) ;
#741 = EDGE_CURVE ( 'NONE', #9183, #17652, #3050, .T. ) ;
#742 = LINE ( 'NONE', #15203, #4415 ) ;
#743 = ORIENTED_EDGE ( 'NONE', *, *, #1591, .T. ) ;
#744 = PLANE ( 'NONE',  #2004 ) ;
#745 = LINE ( 'NONE', #12048, #16067 ) ;
#746 = CARTESIAN_POINT ( 'NONE',  ( -2.137408332595969629, -3.450151633892079683, 3.714996798363980002 ) ) ;
#747 = VERTEX_POINT ( 'NONE', #8341 ) ;
#748 = EDGE_LOOP ( 'NONE', ( #6942, #11211, #13896, #14594, #10227, #13721, #1763, #3427, #3347, #8912, #16607, #3116, #1632, #10771, #8081, #10005 ) ) ;
#749 = CARTESIAN_POINT ( 'NONE',  ( 1.899999999999999911, 11.40000000000000036, 0.5999999999999999778 ) ) ;
#750 = ORIENTED_EDGE ( 'NONE', *, *, #6537, .T. ) ;
#751 = CARTESIAN_POINT ( 'NONE',  ( -1.199999999999880052, 11.40000000000000036, -2.399999999999999911 ) ) ;
#752 = APPLICATION_PROTOCOL_DEFINITION ( 'draft international standard', 'automotive_design', 1998, #16913 ) ;
#753 = CARTESIAN_POINT ( 'NONE',  ( 2.043308330018790198, -5.099788135593220417, 5.867646457774659652 ) ) ;
#754 = EDGE_CURVE ( 'NONE', #2115, #2289, #6939, .T. ) ;
#755 = CARTESIAN_POINT ( 'NONE',  ( 1.800000000000000044, 0.5999999999999999778, 7.599999999999999645 ) ) ;
#756 = ORIENTED_EDGE ( 'NONE', *, *, #4010, .F. ) ;
#757 = AXIS2_PLACEMENT_3D ( 'NONE', #3636, #9288, #13742 ) ;
#758 = EDGE_CURVE ( 'NONE', #16493, #14177, #16933, .T. ) ;
#759 = CARTESIAN_POINT ( 'NONE',  ( -0.5972539422561604638, -4.591277760018214416, 6.664227474374482263 ) ) ;
#760 = EDGE_CURVE ( 'NONE', #2828, #7698, #4894, .T. ) ;
#761 = EDGE_CURVE ( 'NONE', #3042, #17417, #10351, .T. ) ;
#762 = CARTESIAN_POINT ( 'NONE',  ( -1.031876288691620625, -0.4690677966101705065, 7.145012538880312292 ) ) ;
#763 = ORIENTED_EDGE ( 'NONE', *, *, #1986, .F. ) ;
#764 = ADVANCED_FACE ( 'NONE', ( #4594 ), #2377, .T. ) ;
#765 = CARTESIAN_POINT ( 'NONE',  ( 1.248294325655350034, -0.02669491525423759934, 2.704938983774300088 ) ) ;
#766 = AXIS2_PLACEMENT_3D ( 'NONE', #8146, #9443, #5172 ) ;
#767 = ORIENTED_EDGE ( 'NONE', *, *, #5410, .F. ) ;
#768 = LINE ( 'NONE', #17692, #2401 ) ;
#769 = FACE_OUTER_BOUND ( 'NONE', #9696, .T. ) ;
#770 = VECTOR ( 'NONE', #4515, 1000.000000000000000 ) ;
#771 = VECTOR ( 'NONE', #10141, 1000.000000000000000 ) ;
#772 = CARTESIAN_POINT ( 'NONE',  ( -0.4005155088301870503, -1.125163681423229978, 7.019123328904779413 ) ) ;
#773 = CARTESIAN_POINT ( 'NONE',  ( 1.791574935211219799, -5.408686440677969998, 6.226029630577610163 ) ) ;
#774 = CARTESIAN_POINT ( 'NONE',  ( 2.652408070456659051, -0.6826862039457533005, 4.611427313555195084 ) ) ;
#775 = ORIENTED_EDGE ( 'NONE', *, *, #17107, .T. ) ;
#776 = CARTESIAN_POINT ( 'NONE',  ( 1.889999999999999902, 8.500000000000000000, 0.5999999999999999778 ) ) ;
#777 = CARTESIAN_POINT ( 'NONE',  ( 0.8429265834919229539, -3.523857375116919766, 2.502678798553439776 ) ) ;
#778 = CARTESIAN_POINT ( 'NONE',  ( -1.835211330903778970, -4.707719201459645397, 6.617058440404012032 ) ) ;
#779 = DIRECTION ( 'NONE',  ( 7.401486830834380223E-16, -4.695600626315549922E-31, 1.000000000000000000 ) ) ;
#780 = CARTESIAN_POINT ( 'NONE',  ( 0.1749999999999999889, 7.900000000000000355, 0.4000000000000000222 ) ) ;
#782 = EDGE_CURVE ( 'NONE', #17164, #14972, #13576, .T. ) ;
#781 = FACE_OUTER_BOUND ( 'NONE', #12825, .T. ) ;
#783 = CARTESIAN_POINT ( 'NONE',  ( 1.889999999999999902, 3.500000000000000000, -6.651892103230508783E-16 ) ) ;
#784 = AXIS2_PLACEMENT_3D ( 'NONE', #4287, #7263, #3090 ) ;
#785 = CARTESIAN_POINT ( 'NONE',  ( -0.7128755192781907057, -1.777235753495299608, 2.774718115017459130 ) ) ;
#786 = VERTEX_POINT ( 'NONE', #7488 ) ;
#787 = FACE_OUTER_BOUND ( 'NONE', #15263, .T. ) ;
#788 = LINE ( 'NONE', #12185, #4394 ) ;
#789 = CARTESIAN_POINT ( 'NONE',  ( -2.282375681463830297, -3.174533050792599731, 3.345793611865449435 ) ) ;
#790 = ORIENTED_EDGE ( 'NONE', *, *, #5174, .T. ) ;
#791 = FACE_OUTER_BOUND ( 'NONE', #7316, .T. ) ;
#792 = CARTESIAN_POINT ( 'NONE',  ( 2.350542563031990273, -1.004881363621820123, 4.817027120179740329 ) ) ;
#793 = VECTOR ( 'NONE', #16639, 1000.000000000000000 ) ;
#794 = CARTESIAN_POINT ( 'NONE',  ( 2.030998484741458832, -5.081991525423726230, 4.999543428097175557 ) ) ;
#795 = EDGE_LOOP ( 'NONE', ( #2285, #12347, #15673, #9124 ) ) ;
#796 = VERTEX_POINT ( 'NONE', #890 ) ;
#797 = LINE ( 'NONE', #17727, #12065 ) ;
#798 = CARTESIAN_POINT ( 'NONE',  ( -1.399999999999999911, -7.000000000000000000, 3.299999999999999822 ) ) ;
#799 = ORIENTED_EDGE ( 'NONE', *, *, #16349, .F. ) ;
#800 = VECTOR ( 'NONE', #5463, 1000.000000000000000 ) ;
#801 = CARTESIAN_POINT ( 'NONE',  ( -0.5664586606772434862, -5.286652542372874741, 2.726727161522279452 ) ) ;
#802 = VECTOR ( 'NONE', #10018, 1000.000000000000000 ) ;
#803 = AXIS2_PLACEMENT_3D ( 'NONE', #17116, #7059, #2881 ) ;
#804 = CARTESIAN_POINT ( 'NONE',  ( 1.071153154657499718, -2.545749267008810435, 7.128115444592616257 ) ) ;
#805 = CARTESIAN_POINT ( 'NONE',  ( 0.2435295127647319202, -5.004947479095227969, 2.350795284704489507 ) ) ;
#806 = CARTESIAN_POINT ( 'NONE',  ( 1.991177874369370882, -2.378890372630820149, 2.945484578117438801 ) ) ;
#807 = FACE_OUTER_BOUND ( 'NONE', #12417, .T. ) ;
#808 = LINE ( 'NONE', #6450, #6415 ) ;
#809 = VECTOR ( 'NONE', #12432, 1000.000000000000000 ) ;
#810 = CARTESIAN_POINT ( 'NONE',  ( -1.480680413335760059, -4.385524041783589233, 6.529298007719829933 ) ) ;
#811 = CIRCLE ( 'NONE', #6130, 0.1499999999999999667 ) ;
#812 = VECTOR ( 'NONE', #1415, 1000.000000000000000 ) ;
#813 = ADVANCED_FACE ( 'NONE', ( #14435 ), #10252, .T. ) ;
#814 = DIRECTION ( 'NONE',  ( 6.123233995736806712E-17, 0.000000000000000000, 1.000000000000000000 ) ) ;
#816 = ORIENTED_EDGE ( 'NONE', *, *, #17509, .T. ) ;
#815 = CARTESIAN_POINT ( 'NONE',  ( 2.146130664537611032, -2.402178660919109365, 3.138834773724044958 ) ) ;
#817 = AXIS2_PLACEMENT_3D ( 'NONE', #12785, #1981, #10411 ) ;
#818 = DIRECTION ( 'NONE',  ( 1.000000000000000000, 3.315303352997239924E-31, 0.000000000000000000 ) ) ;
#819 = AXIS2_PLACEMENT_3D ( 'NONE', #1636, #253, #11619 ) ;
#820 = CARTESIAN_POINT ( 'NONE',  ( 0.8570167067220200163, -0.3177966101694920664, 2.508190348879349774 ) ) ;
#821 = CARTESIAN_POINT ( 'NONE',  ( -1.741913176380149864, -1.959701183441629802, 3.117443785062560035 ) ) ;
#822 = CARTESIAN_POINT ( 'NONE',  ( -1.811729841638700211, -0.5580508474576270084, 3.197954009834299782 ) ) ;
#823 = LINE ( 'NONE', #6464, #13603 ) ;
#824 = EDGE_LOOP ( 'NONE', ( #15107, #16470, #568, #13760, #3592, #3599, #8119, #9168, #15975 ) ) ;
#825 = ORIENTED_EDGE ( 'NONE', *, *, #18216, .F. ) ;
#826 = CARTESIAN_POINT ( 'NONE',  ( 0.4974685680287857514, -5.139830508474579673, 7.000224381598740386 ) ) ;
#827 = PLANE ( 'NONE',  #9362 ) ;
#828 = DIRECTION ( 'NONE',  ( 0.000000000000000000, 0.000000000000000000, -1.000000000000000000 ) ) ;
#829 = VECTOR ( 'NONE', #11921, 1000.000000000000000 ) ;
#830 = APPLICATION_CONTEXT ( 'automotive_design' ) ;
#831 = VECTOR ( 'NONE', #2430, 1000.000000000000000 ) ;
#832 = EDGE_LOOP ( 'NONE', ( #16640, #4367, #7529, #3942 ) ) ;
#833 = CARTESIAN_POINT ( 'NONE',  ( 2.276802572547980130, -2.495331814072260013, 4.104251954998760610 ) ) ;
#834 = PLANE ( 'NONE',  #8219 ) ;
#835 = CARTESIAN_POINT ( 'NONE',  ( -2.353194804772640314, -5.524364406779660008, 4.731327187377240229 ) ) ;
#836 = AXIS2_PLACEMENT_3D ( 'NONE', #6620, #6332, #10894 ) ;
#837 = CARTESIAN_POINT ( 'NONE',  ( -1.899999999999999911, 7.299999999999999822, 1.600000000000000089 ) ) ;
#838 = CARTESIAN_POINT ( 'NONE',  ( 2.075124426334590044, -2.681638120378570189, 5.810227140144509583 ) ) ;
#839 = VECTOR ( 'NONE', #14410, 1000.000000000000000 ) ;
#840 = DIRECTION ( 'NONE',  ( 0.7071067811865594521, 0.000000000000000000, 0.7071067811865355823 ) ) ;
#841 = AXIS2_PLACEMENT_3D ( 'NONE', #7581, #9048, #2022 ) ;
#842 = CARTESIAN_POINT ( 'NONE',  ( -0.5133516189064535329, -1.447358841099289251, 6.687805814961367723 ) ) ;
#843 = CARTESIAN_POINT ( 'NONE',  ( 0.8740908734716299477, 4.154758922476410099, 7.700000000000000178 ) ) ;
#844 = DIRECTION ( 'NONE',  ( 3.172065784643300034E-16, -1.000000000000000000, -1.586032892321649771E-16 ) ) ;
#845 = ORIENTED_EDGE ( 'NONE', *, *, #5292, .F. ) ;
#846 = CARTESIAN_POINT ( 'NONE',  ( 1.668386990667991565, -0.4963805274437239623, 3.049705503900983938 ) ) ;
#847 = AXIS2_PLACEMENT_3D ( 'NONE', #1522, #3164, #11588 ) ;
#848 = CARTESIAN_POINT ( 'NONE',  ( -1.899999999999999911, 10.00000000000000000, 6.661338147750939243E-16 ) ) ;
#849 = CARTESIAN_POINT ( 'NONE',  ( -1.948278411993560111, -3.193980462720909852, 6.020210936496040333 ) ) ;
#850 = ORIENTED_EDGE ( 'NONE', *, *, #14353, .T. ) ;
#851 = VERTEX_POINT ( 'NONE', #541 ) ;
#852 = DIRECTION ( 'NONE',  ( 0.000000000000000000, 0.000000000000000000, 1.000000000000000000 ) ) ;
#853 = SHAPE_REPRESENTATION ( 'Solder Terminal Pins', ( #17681 ), #4692 ) ;
#854 = ORIENTED_EDGE ( 'NONE', *, *, #7368, .F. ) ;
#855 = DIRECTION ( 'NONE',  ( -1.000000000000000000, 7.401486830834380223E-16, 0.000000000000000000 ) ) ;
#856 = VECTOR ( 'NONE', #9398, 1000.000000000000000 ) ;
#857 = CARTESIAN_POINT ( 'NONE',  ( 2.328217775191430139, -5.081991525423729783, 5.043379051721160522 ) ) ;
#858 = VECTOR ( 'NONE', #4451, 1000.000000000000000 ) ;
#859 = ORIENTED_EDGE ( 'NONE', *, *, #8286, .F. ) ;
#860 = CARTESIAN_POINT ( 'NONE',  ( -2.313035575219740014, -1.427911429170980018, 5.134294963419759661 ) ) ;
#861 =( GEOMETRIC_REPRESENTATION_CONTEXT ( 3 ) GLOBAL_UNCERTAINTY_ASSIGNED_CONTEXT ( ( #13984 ) ) GLOBAL_UNIT_ASSIGNED_CONTEXT ( ( #312, #15598, #45 ) ) REPRESENTATION_CONTEXT ( 'NONE', 'WORKASPACE' ) );
#862 = DIRECTION ( 'NONE',  ( 1.708035422500239940E-16, -1.000000000000000000, -4.270088556250599234E-17 ) ) ;
#863 = CARTESIAN_POINT ( 'NONE',  ( 1.224086244040949900, -4.358394877135324030, 6.348185277745746369 ) ) ;
#864 = CARTESIAN_POINT ( 'NONE',  ( 2.253200202764420013, -0.08898305084745811167, 5.379408587037500133 ) ) ;
#865 = ORIENTED_EDGE ( 'NONE', *, *, #17396, .T. ) ;
#866 = CARTESIAN_POINT ( 'NONE',  ( 2.318251751302029984, -0.3667372881355940306, 4.294764266798990704 ) ) ;
#867 = AXIS2_PLACEMENT_3D ( 'NONE', #11342, #16977, #4289 ) ;
#868 = CARTESIAN_POINT ( 'NONE',  ( 1.347262683220810553, -0.1245762711864410871, 6.986424775243341045 ) ) ;
#869 = ORIENTED_EDGE ( 'NONE', *, *, #1000, .F. ) ;
#870 = CARTESIAN_POINT ( 'NONE',  ( -2.306642602145299925, -5.515466101694909362, 5.166805192608490138 ) ) ;
#871 = DIRECTION ( 'NONE',  ( 9.588835100573269740E-31, -1.000000000000000000, -3.548581835996780230E-45 ) ) ;
#872 = CARTESIAN_POINT ( 'NONE',  ( 1.914021115237029225, -0.8457042219637708191, 6.069404563272199127 ) ) ;
#873 = CARTESIAN_POINT ( 'NONE',  ( 1.112838723655040107, -5.426483050847459744, 6.773667561836210105 ) ) ;
#874 = EDGE_CURVE ( 'NONE', #7005, #8096, #1357, .T. ) ;
#875 = CARTESIAN_POINT ( 'NONE',  ( -2.501774541437291610, -4.824160642901089702, 5.585572039315926496 ) ) ;
#876 = ORIENTED_EDGE ( 'NONE', *, *, #12310, .F. ) ;
#877 = CARTESIAN_POINT ( 'NONE',  ( 0.3042893218813449985, 3.050000000000000266, 2.170710678118660031 ) ) ;
#878 = EDGE_CURVE ( 'NONE', #4810, #396, #13218, .T. ) ;
#879 = AXIS2_PLACEMENT_3D ( 'NONE', #3054, #10353, #4601 ) ;
#880 = CARTESIAN_POINT ( 'NONE',  ( 2.267872052190590182, -3.756740257999799937, 4.071110468860600129 ) ) ;
#881 = EDGE_CURVE ( 'NONE', #458, #14474, #12272, .T. ) ;
#882 = CARTESIAN_POINT ( 'NONE',  ( 1.373536515609961484, -4.381683165423609694, 6.970795264502707589 ) ) ;
#883 = CARTESIAN_POINT ( 'NONE',  ( 2.616666666666660035, -5.805074450128190455E-17, 4.000000000000000000 ) ) ;
#884 = LINE ( 'NONE', #9578, #15287 ) ;
#885 = CARTESIAN_POINT ( 'NONE',  ( 2.052909741356249373, -3.826605122864674247, 4.721527574705135066 ) ) ;
#886 = DIRECTION ( 'NONE',  ( -1.000000000000000000, 0.000000000000000000, 0.000000000000000000 ) ) ;
#887 = DIRECTION ( 'NONE',  ( 0.000000000000000000, 0.000000000000000000, -1.000000000000000000 ) ) ;
#888 = CARTESIAN_POINT ( 'NONE',  ( 0.2220816246932099114, -1.055298816558370101, 6.740975647723836950 ) ) ;
#889 = ORIENTED_EDGE ( 'NONE', *, *, #3094, .F. ) ;
#890 = CARTESIAN_POINT ( 'NONE',  ( 0.2750000000000004663, 2.299999999999999822, 7.700000000000000178 ) ) ;
#891 = DIRECTION ( 'NONE',  ( -3.172065784643300034E-16, 1.000000000000000000, 0.000000000000000000 ) ) ;
#892 = LINE ( 'NONE', #17525, #2014 ) ;
#893 = CARTESIAN_POINT ( 'NONE',  ( 1.503451935564949826, -2.499172690432241772, 6.886949009567407742 ) ) ;
#894 = ORIENTED_EDGE ( 'NONE', *, *, #5217, .T. ) ;
#895 = CIRCLE ( 'NONE', #17419, 0.5500000000000001554 ) ;
#896 = PLANE ( 'NONE',  #3171 ) ;
#897 = CARTESIAN_POINT ( 'NONE',  ( -1.399999999999999911, -9.500000000000000000, 6.100000000000000533 ) ) ;
#898 = DIRECTION ( 'NONE',  ( -0.9622640697945192834, -0.2721173643531198949, 0.000000000000000000 ) ) ;
#899 = CARTESIAN_POINT ( 'NONE',  ( 1.940327948426050941, -5.090889830508485758, 5.370677689277660427 ) ) ;
#900 = EDGE_LOOP ( 'NONE', ( #8185, #16443, #4602, #11112 ) ) ;
#901 = ORIENTED_EDGE ( 'NONE', *, *, #754, .F. ) ;
#902 = CARTESIAN_POINT ( 'NONE',  ( 8.549934884138839976E-16, 6.262741699796950279, 6.100000000000000533 ) ) ;
#903 = PLANE ( 'NONE',  #13840 ) ;
#904 = FACE_OUTER_BOUND ( 'NONE', #4232, .T. ) ;
#905 = ADVANCED_FACE ( 'NONE', ( #3231, #6187, #7405, #8875 ), #11842, .T. ) ;
#906 = ORIENTED_EDGE ( 'NONE', *, *, #4194, .T. ) ;
#907 = CARTESIAN_POINT ( 'NONE',  ( -0.3743405594629430344, -5.457627118644070130, 7.023440622744399953 ) ) ;
#908 = CARTESIAN_POINT ( 'NONE',  ( -1.923406176634930853, -4.796950468210009255, 2.875176962145308934 ) ) ;
#909 = PLANE ( 'NONE',  #1757 ) ;
#910 = CYLINDRICAL_SURFACE ( 'NONE', #6751, 0.3999999999999999667 ) ;
#911 = CARTESIAN_POINT ( 'NONE',  ( -1.800000000000000044, 3.552713678800499647E-16, 9.441371669411539713 ) ) ;
#912 = VECTOR ( 'NONE', #3016, 1000.000000000000000 ) ;
#913 = CARTESIAN_POINT ( 'NONE',  ( 0.2023972492402060230, -3.453992510252060111, 2.355265251465770149 ) ) ;
#914 = DIRECTION ( 'NONE',  ( -1.000000000000000000, 1.153478467143200106E-14, -8.997169018144999103E-17 ) ) ;
#915 = CARTESIAN_POINT ( 'NONE',  ( 0.1749999999999999889, 9.500000000000000000, 3.100000000000000089 ) ) ;
#917 = VERTEX_POINT ( 'NONE', #448 ) ;
#916 = CARTESIAN_POINT ( 'NONE',  ( -2.121170185508219230, -1.936412895153350133, 3.105085978143999448 ) ) ;
#918 = DIRECTION ( 'NONE',  ( -1.000000000000000000, 0.000000000000000000, 1.268826313857320014E-15 ) ) ;
#919 = DIRECTION ( 'NONE',  ( -1.000000000000000000, 0.000000000000000000, 0.000000000000000000 ) ) ;
#920 = CARTESIAN_POINT ( 'NONE',  ( -1.003115764947269950, -1.493935417675869903, 6.828967930617589666 ) ) ;
#921 = CARTESIAN_POINT ( 'NONE',  ( -0.002227590684729350255, -5.185305426092289949, 2.202374039106770098 ) ) ;
#922 = CARTESIAN_POINT ( 'NONE',  ( -2.253200202764409799, -5.511016949152540256, 5.379408587037509903 ) ) ;
#923 = ORIENTED_EDGE ( 'NONE', *, *, #17952, .T. ) ;
#924 = ORIENTED_EDGE ( 'NONE', *, *, #12319, .F. ) ;
#925 = DIRECTION ( 'NONE',  ( -1.000000000000000000, 0.000000000000000000, 0.000000000000000000 ) ) ;
#926 = AXIS2_PLACEMENT_3D ( 'NONE', #3855, #2475, #9213 ) ;
#927 = DIRECTION ( 'NONE',  ( 7.656710514656250048E-17, -0.9659258262890690894, -0.2588190451025180749 ) ) ;
#928 = ADVANCED_FACE ( 'NONE', ( #15069 ), #16017, .F. ) ;
#929 = ORIENTED_EDGE ( 'NONE', *, *, #3392, .F. ) ;
#930 = CARTESIAN_POINT ( 'NONE',  ( 2.190084968185480374, -4.032358841099290103, 3.838447030292440054 ) ) ;
#931 = FACE_OUTER_BOUND ( 'NONE', #3401, .T. ) ;
#932 = CARTESIAN_POINT ( 'NONE',  ( -0.1565249325564300187, -5.453177966101690366, 7.048192310558509810 ) ) ;
#933 = CARTESIAN_POINT ( 'NONE',  ( 0.02999999999999939868, 12.00000000000000000, 1.600000000000000089 ) ) ;
#934 = ADVANCED_FACE ( 'NONE', ( #11744 ), #8962, .T. ) ;
#935 = CARTESIAN_POINT ( 'NONE',  ( -0.09706517602693919000, -2.961097579838030125, 7.051451474958980725 ) ) ;
#936 = CARTESIAN_POINT ( 'NONE',  ( 0.5000000000000000000, 4.631370849898480024, 5.100000000000000533 ) ) ;
#937 = CARTESIAN_POINT ( 'NONE',  ( 1.259207372045950457, -2.332313796054251487, 3.078488779929903441 ) ) ;
#938 = DIRECTION ( 'NONE',  ( -1.734723475976809806E-16, 1.000000000000000000, 6.938893903907229610E-17 ) ) ;
#939 = CARTESIAN_POINT ( 'NONE',  ( -0.009452110982655715157, -0.5998079552954631577, 2.050000000000001155 ) ) ;
#940 = ORIENTED_EDGE ( 'NONE', *, *, #5197, .F. ) ;
#941 = CARTESIAN_POINT ( 'NONE',  ( 1.561564427405139899, -5.242163535134220176, 3.138435572594850065 ) ) ;
#942 = DIRECTION ( 'NONE',  ( -1.850371707708589879E-16, 1.000000000000000000, 0.000000000000000000 ) ) ;
#943 = DIRECTION ( 'NONE',  ( 1.000000000000000000, 0.000000000000000000, 0.000000000000000000 ) ) ;
#944 = ORIENTED_EDGE ( 'NONE', *, *, #11615, .T. ) ;
#945 = ORIENTED_EDGE ( 'NONE', *, *, #2348, .T. ) ;
#946 = DIRECTION ( 'NONE',  ( 2.220446049250309876E-16, 1.110223024625159992E-16, -1.000000000000000000 ) ) ;
#947 = ADVANCED_FACE ( 'NONE', ( #4699 ), #14962, .T. ) ;
#948 = ORIENTED_EDGE ( 'NONE', *, *, #11855, .F. ) ;
#949 = CARTESIAN_POINT ( 'NONE',  ( -0.3042893218813459977, 6.450000000000000178, 2.029289321881350361 ) ) ;
#950 = CARTESIAN_POINT ( 'NONE',  ( 2.350067830300900162, -5.077542372881360677, 4.825253242917690422 ) ) ;
#951 = CARTESIAN_POINT ( 'NONE',  ( 2.500000000000000000, 4.700000000000000178, 1.600000000000000089 ) ) ;
#952 = DIRECTION ( 'NONE',  ( 1.060879779086260081E-14, -8.223874256482640091E-16, 1.000000000000000000 ) ) ;
#953 = ORIENTED_EDGE ( 'NONE', *, *, #17999, .F. ) ;
#954 = CARTESIAN_POINT ( 'NONE',  ( -2.579602008086729459, -4.548542059801595094, 5.323511966907305215 ) ) ;
#955 = LINE ( 'NONE', #3904, #15604 ) ;
#956 = CARTESIAN_POINT ( 'NONE',  ( -1.586727176531439909, -1.982989471729919906, 2.961885344765640138 ) ) ;
#957 = VECTOR ( 'NONE', #14005, 1000.000000000000000 ) ;
#958 = CARTESIAN_POINT ( 'NONE',  ( 1.378221871957440170, -0.1201271186440679983, 6.607619368096269596 ) ) ;
#959 = VERTEX_POINT ( 'NONE', #2271 ) ;
#960 = CARTESIAN_POINT ( 'NONE',  ( -2.508228811380011081, -0.2091101694915259990, 5.566973598334550744 ) ) ;
#961 = ORIENTED_EDGE ( 'NONE', *, *, #14653, .T. ) ;
#962 = PLANE ( 'NONE',  #17086 ) ;
#963 = CARTESIAN_POINT ( 'NONE',  ( -2.313035575219740014, -1.427911429170980240, 5.134294963419758773 ) ) ;
#964 = CARTESIAN_POINT ( 'NONE',  ( -1.496290472746829803, -0.5672554343907050267, 2.872674968141029961 ) ) ;
#965 = CARTESIAN_POINT ( 'NONE',  ( 2.051568858000881068, -0.5196681859277345605, 3.016498023208322277 ) ) ;
#966 = ORIENTED_EDGE ( 'NONE', *, *, #8760, .T. ) ;
#967 = CARTESIAN_POINT ( 'NONE',  ( -1.314185150718290895, -5.128627060139315574, 3.113044112970123400 ) ) ;
#968 = AXIS2_PLACEMENT_3D ( 'NONE', #5506, #11151, #6990 ) ;
#969 = CARTESIAN_POINT ( 'NONE',  ( 1.953802435660499048, -0.6128213390808875394, 4.069478085300975323 ) ) ;
#970 = CARTESIAN_POINT ( 'NONE',  ( -2.652408070456659051, -4.917313796054240349, 4.611427313555255481 ) ) ;
#971 = CARTESIAN_POINT ( 'NONE',  ( 1.899999999999999911, 11.15000000000000036, 1.600000000000000089 ) ) ;
#972 = DIRECTION ( 'NONE',  ( 2.220446049250309876E-16, 1.000000000000000000, 1.479114197289400113E-30 ) ) ;
#973 = CARTESIAN_POINT ( 'NONE',  ( -1.978802102381380879, -1.843259742000191048, 4.152967933079680485 ) ) ;
#974 = CARTESIAN_POINT ( 'NONE',  ( -1.000000000000000000, 5.400000000000000355, 7.700000000000000178 ) ) ;
#975 = FACE_OUTER_BOUND ( 'NONE', #1124, .T. ) ;
#976 = CARTESIAN_POINT ( 'NONE',  ( -0.3943683997330095781, -3.384127645387192018, 2.685210827922659860 ) ) ;
#977 = ORIENTED_EDGE ( 'NONE', *, *, #1593, .F. ) ;
#978 = CARTESIAN_POINT ( 'NONE',  ( -1.399999999999999911, -5.500000000000000000, 6.100000000000000533 ) ) ;
#979 = PLANE ( 'NONE',  #13237 ) ;
#980 = CARTESIAN_POINT ( 'NONE',  ( -0.7982439214406890082, -0.1690677966101698793, 6.591424794228156081 ) ) ;
#981 = CARTESIAN_POINT ( 'NONE',  ( 1.139503474074560874, -0.7471169921413568504, 2.982738323988489260 ) ) ;
#982 = CARTESIAN_POINT ( 'NONE',  ( 2.327043743583509627, -2.382731248990799244, 5.975923629552606364 ) ) ;
#983 = EDGE_CURVE ( 'NONE', #389, #13368, #12182, .T. ) ;
#984 = ORIENTED_EDGE ( 'NONE', *, *, #10962, .F. ) ;
#985 = DIRECTION ( 'NONE',  ( 1.000000000000000000, 1.908195823574489776E-16, 1.110223024625159992E-16 ) ) ;
#986 = CARTESIAN_POINT ( 'NONE',  ( -0.5137283630188880235, -5.162076271186444743, 6.687652957477222770 ) ) ;
#987 = ORIENTED_EDGE ( 'NONE', *, *, #1836, .T. ) ;
#988 = ORIENTED_EDGE ( 'NONE', *, *, #7143, .F. ) ;
#989 = CARTESIAN_POINT ( 'NONE',  ( -1.399999999999999911, -8.000000000000000000, 3.299999999999999822 ) ) ;
#990 = CARTESIAN_POINT ( 'NONE',  ( 1.699999999999999956, 9.299999999999998934, 7.599999999999999645 ) ) ;
#991 = CARTESIAN_POINT ( 'NONE',  ( -2.350000000000000089, -5.599999999999999645, 6.400000000000000355 ) ) ;
#992 = ORIENTED_EDGE ( 'NONE', *, *, #2120, .F. ) ;
#993 = CARTESIAN_POINT ( 'NONE',  ( 1.925796468768800063, -5.404237288135590234, 6.052706598917719560 ) ) ;
#994 = CARTESIAN_POINT ( 'NONE',  ( -2.650521604678268694, -4.595118636378185073, 4.833599835830360014 ) ) ;
#995 = FACE_OUTER_BOUND ( 'NONE', #6865, .T. ) ;
#996 = CARTESIAN_POINT ( 'NONE',  ( -1.837442528958838750, -3.543304787045241433, 2.785079989718828752 ) ) ;
#997 = CARTESIAN_POINT ( 'NONE',  ( -1.800000000000000044, 12.00000000000000000, 1.600000000000000089 ) ) ;
#998 = CARTESIAN_POINT ( 'NONE',  ( -1.444955263746759977, -3.267686203945750378, 2.842353646881510265 ) ) ;
#999 = CARTESIAN_POINT ( 'NONE',  ( 0.4000000000000000222, -1.399999999999999911, 6.100000000000000533 ) ) ;
#1000 = EDGE_CURVE ( 'NONE', #11463, #8080, #17800, .T. ) ;
#1001 = DIRECTION ( 'NONE',  ( -1.708035422500239940E-16, 1.000000000000000000, 0.000000000000000000 ) ) ;
#1003 = ORIENTED_EDGE ( 'NONE', *, *, #5108, .T. ) ;
#1002 = CARTESIAN_POINT ( 'NONE',  ( 2.567863625471588751, -2.495331814072259569, 4.029783546918046078 ) ) ;
#1004 = ADVANCED_FACE ( 'NONE', ( #8197 ), #12459, .T. ) ;
#1005 = EDGE_CURVE ( 'NONE', #4096, #12326, #14856, .T. ) ;
#1006 = FACE_OUTER_BOUND ( 'NONE', #2160, .T. ) ;
#1007 = CARTESIAN_POINT ( 'NONE',  ( 2.203023580853990193, -0.3578389830508479919, 3.872235369154280349 ) ) ;
#1008 = ADVANCED_FACE ( 'NONE', ( #15154 ), #13845, .T. ) ;
#1009 = CARTESIAN_POINT ( 'NONE',  ( -1.552749016687749783, -1.563800282540730002, 6.468535037441760061 ) ) ;
#1010 = CARTESIAN_POINT ( 'NONE',  ( -1.641808337277740115, -0.4868644067796619734, 6.386111670537629514 ) ) ;
#1011 = CARTESIAN_POINT ( 'NONE',  ( 2.500000000000000000, 8.500000000000000000, 0.6099999999999999867 ) ) ;
#1012 = CARTESIAN_POINT ( 'NONE',  ( 2.171642826483958899, -5.404237288135596451, 6.225392547715717484 ) ) ;
#1013 = ORIENTED_EDGE ( 'NONE', *, *, #1671, .F. ) ;
#1014 = CARTESIAN_POINT ( 'NONE',  ( -1.889999999999999902, 8.500000000000000000, 2.702225438111990169E-15 ) ) ;
#1015 = CARTESIAN_POINT ( 'NONE',  ( 2.224278379903029457, -5.090889830508479541, 5.468825643806100700 ) ) ;
#1016 = CARTESIAN_POINT ( 'NONE',  ( 0.5500000000000000444, 7.799999999999999822, 3.600000000000000089 ) ) ;
#1017 = PLANE ( 'NONE',  #2330 ) ;
#1018 = ORIENTED_EDGE ( 'NONE', *, *, #16662, .T. ) ;
#1019 = CARTESIAN_POINT ( 'NONE',  ( -0.04278372834682089842, -3.729611093351540063, 2.346934926511239805 ) ) ;
#1020 = CARTESIAN_POINT ( 'NONE',  ( 0.6500000000000000222, 3.050000000000000266, 2.699264068711930253 ) ) ;
#1021 = CARTESIAN_POINT ( 'NONE',  ( -0.07299321914061848715, -5.598516949152539723, 2.350000000000000089 ) ) ;
#1022 = AXIS2_PLACEMENT_3D ( 'NONE', #2980, #8623, #3057 ) ;
#1023 = FACE_OUTER_BOUND ( 'NONE', #9086, .T. ) ;
#1024 = DIRECTION ( 'NONE',  ( -1.903239470785979823E-16, -1.000000000000000000, 0.000000000000000000 ) ) ;
#1025 = CARTESIAN_POINT ( 'NONE',  ( 1.444955263746720009, -2.332313796054249710, 2.842353646881480511 ) ) ;
#1026 = CARTESIAN_POINT ( 'NONE',  ( -1.209303714320900225, -4.865515740159330527, 2.662663894020050659 ) ) ;
#1027 = CARTESIAN_POINT ( 'NONE',  ( 1.893291846171430981, -2.658349832090279197, 5.493944474033856551 ) ) ;
#1028 = EDGE_CURVE ( 'NONE', #13803, #4524, #15525, .T. ) ;
#1029 = PLANE ( 'NONE',  #13544 ) ;
#1030 = CARTESIAN_POINT ( 'NONE',  ( 0.6493550500446280127, -0.3133474576271190193, 2.437955526623099889 ) ) ;
#1031 = CARTESIAN_POINT ( 'NONE',  ( -2.500000000000000000, 7.299999999999999822, 1.600000000000000089 ) ) ;
#1032 = ORIENTED_EDGE ( 'NONE', *, *, #16095, .F. ) ;
#1033 = CARTESIAN_POINT ( 'NONE',  ( -1.149999999999999911, 9.274118095489749081, 7.596592582628910684 ) ) ;
#1034 = CARTESIAN_POINT ( 'NONE',  ( -1.820241257191459905, -5.080331814072259533, 3.208199930689799917 ) ) ;
#1035 = STYLED_ITEM ( 'NONE', ( #2676 ), #2155 ) ;
#1036 = ORIENTED_EDGE ( 'NONE', *, *, #7213, .F. ) ;
#1037 = ORIENTED_EDGE ( 'NONE', *, *, #9794, .T. ) ;
#1038 = UNCERTAINTY_MEASURE_WITH_UNIT (LENGTH_MEASURE( 1.000000000000000082E-05 ), #15942, 'distance_accuracy_value', 'NONE');
#1039 = VERTEX_POINT ( 'NONE', #11061 ) ;
#1040 = CARTESIAN_POINT ( 'NONE',  ( -1.875000000000000000, 11.25000000000000000, 7.700000000000000178 ) ) ;
#1041 = CARTESIAN_POINT ( 'NONE',  ( -1.750316316486840051, -5.259957627118650336, 3.126818518378589928 ) ) ;
#1042 = EDGE_CURVE ( 'NONE', #16733, #8528, #14114, .T. ) ;
#1043 = CARTESIAN_POINT ( 'NONE',  ( -0.2335786437626909962, 6.450000000000000178, 2.241421356237310203 ) ) ;
#1044 = ORIENTED_EDGE ( 'NONE', *, *, #12721, .F. ) ;
#1045 = CARTESIAN_POINT ( 'NONE',  ( 2.325590009395039903, -0.7292627805223299564, 5.061077271074021056 ) ) ;
#1046 = DIRECTION ( 'NONE',  ( 0.000000000000000000, -1.000000000000000000, 0.000000000000000000 ) ) ;
#1047 = CARTESIAN_POINT ( 'NONE',  ( 2.291237445532070094, -0.9350164987569499209, 4.162434510291790346 ) ) ;
#1048 = CARTESIAN_POINT ( 'NONE',  ( -1.254903241568450900, -0.1735169491525429541, 7.038391080368498365 ) ) ;
#1049 = EDGE_CURVE ( 'NONE', #18164, #8433, #17791, .T. ) ;
#1050 = EDGE_LOOP ( 'NONE', ( #10330, #2699, #7996, #1910 ) ) ;
#1051 = CARTESIAN_POINT ( 'NONE',  ( 2.306642602145299925, -0.3845338983050849979, 5.166805192608480368 ) ) ;
#1052 = CARTESIAN_POINT ( 'NONE',  ( -0.9150601050661559821, -0.4690677966101700069, 6.868218666554230190 ) ) ;
#1053 = EDGE_LOOP ( 'NONE', ( #17004, #2069, #18120, #9573 ) ) ;
#1054 = CARTESIAN_POINT ( 'NONE',  ( -2.416676968769249090, -0.2046610169491529518, 5.796598111919839980 ) ) ;
#1055 = FACE_OUTER_BOUND ( 'NONE', #2756, .T. ) ;
#1056 = CARTESIAN_POINT ( 'NONE',  ( 2.281778813005790330, -0.7525510688106178403, 5.276394947932119273 ) ) ;
#1057 = CARTESIAN_POINT ( 'NONE',  ( -0.4617942143426889690, -0.5906145504024210569, 2.383143958488499692 ) ) ;
#1058 = CARTESIAN_POINT ( 'NONE',  ( 2.293791554891360551, -0.8224159336754829353, 6.034778631725497000 ) ) ;
#1059 = VERTEX_POINT ( 'NONE', #14024 ) ;
#1060 = CARTESIAN_POINT ( 'NONE',  ( 1.899999999999999911, 7.299999999999999822, 0.6099999999999999867 ) ) ;
#1061 = CARTESIAN_POINT ( 'NONE',  ( 1.458615186838411626, -0.4963798976394455664, 3.259477383973563125 ) ) ;
#1062 = CARTESIAN_POINT ( 'NONE',  ( 1.771358649600380142, -4.335106588847043696, 6.676209054601206283 ) ) ;
#1063 = CARTESIAN_POINT ( 'NONE',  ( 7.233457020361919865E-16, 4.000000000000000000, 6.100000000000000533 ) ) ;
#1064 = CARTESIAN_POINT ( 'NONE',  ( -1.889999999999999902, 3.500000000000000000, 0.6099999999999999867 ) ) ;
#1065 = CARTESIAN_POINT ( 'NONE',  ( 1.998374131852729940, -0.9350164987569505870, 4.229465546630494011 ) ) ;
#1066 = PRODUCT ( 'Plunger Actuator', 'Plunger Actuator', '', ( #10668 ) ) ;
#1067 = FACE_OUTER_BOUND ( 'NONE', #7693, .T. ) ;
#1068 = ORIENTED_EDGE ( 'NONE', *, *, #5750, .F. ) ;
#1069 = FACE_OUTER_BOUND ( 'NONE', #13071, .T. ) ;
#1070 = DIRECTION ( 'NONE',  ( -1.224646799147351975E-16, 1.000000000000000000, 6.123233995736759873E-17 ) ) ;
#1071 = CARTESIAN_POINT ( 'NONE',  ( 0.1910247150515120007, -0.3044491525423730915, 2.655937705488500722 ) ) ;
#1072 = APPLICATION_CONTEXT ( 'automotive_design' ) ;
#1073 = CIRCLE ( 'NONE', #17894, 0.1499999999999999944 ) ;
#1074 = CARTESIAN_POINT ( 'NONE',  ( -2.065789008932981119, -2.871785303044851023, 6.366022047745341084 ) ) ;
#1075 = CARTESIAN_POINT ( 'NONE',  ( -1.850000000000000089, 0.7500000000000000000, 7.649999999999999467 ) ) ;
#1076 = DIRECTION ( 'NONE',  ( 6.123233995736764803E-17, 1.000000000000000000, 0.000000000000000000 ) ) ;
#1077 = CARTESIAN_POINT ( 'NONE',  ( -0.06367493584607197832, -5.298516949152545230, 2.649999999999998579 ) ) ;
#1078 = ORIENTED_EDGE ( 'NONE', *, *, #10764, .F. ) ;
#1079 = LINE ( 'NONE', #17619, #15708 ) ;
#1080 = CARTESIAN_POINT ( 'NONE',  ( 2.286166334984490067, -5.386440677966100488, 5.258525443163859947 ) ) ;
#1081 = DIRECTION ( 'NONE',  ( -1.224646799147350002E-16, 1.000000000000000000, 6.123233995736759873E-17 ) ) ;
#1082 = ORIENTED_EDGE ( 'NONE', *, *, #1809, .T. ) ;
#1083 = CARTESIAN_POINT ( 'NONE',  ( 2.234315482767910144, -5.359745762711869865, 3.960850823455320580 ) ) ;
#1084 = CARTESIAN_POINT ( 'NONE',  ( -2.174104834890490778, -4.455388906648449776, 6.221966445066275497 ) ) ;
#1085 = CLOSED_SHELL ( 'NONE', ( #9768, #689, #15955, #463, #18050, #1932, #10094, #5396, #1581, #3025, #2151, #11551, #5849, #5340, #16454, #1491, #3707, #14394, #14927, #5854 ) ) ;
#1086 = VECTOR ( 'NONE', #16477, 1000.000000000000000 ) ;
#1087 = PLANE ( 'NONE',  #9686 ) ;
#1088 = EDGE_CURVE ( 'NONE', #5474, #13417, #13693, .T. ) ;
#1089 = CARTESIAN_POINT ( 'NONE',  ( 3.179896940101190659E-17, 3.786446520921929793, 7.919316580472860245 ) ) ;
#1090 = LINE ( 'NONE', #16648, #279 ) ;
#1091 = VERTEX_POINT ( 'NONE', #15437 ) ;
#1092 = VECTOR ( 'NONE', #4555, 1000.000000000000000 ) ;
#1093 = CARTESIAN_POINT ( 'NONE',  ( -1.399999999999999911, -5.000000000000000000, 3.299999999999999822 ) ) ;
#1094 = CARTESIAN_POINT ( 'NONE',  ( -2.332582362116870200, -0.5313559322033900578, 4.387643303570819775 ) ) ;
#1095 = CARTESIAN_POINT ( 'NONE',  ( 0.9170541073686970801, -1.284340823081270067, 6.867431071947180499 ) ) ;
#1096 = CARTESIAN_POINT ( 'NONE',  ( -2.351526912647309953, -0.5269067796610169552, 4.606040641882809261 ) ) ;
#1097 = DIRECTION ( 'NONE',  ( -1.899065700016719806E-16, -1.000000000000000000, 0.000000000000000000 ) ) ;
#1098 = CARTESIAN_POINT ( 'NONE',  ( -2.087380238839969593, -5.493220338983046069, 6.338810156469112833 ) ) ;
#1099 = EDGE_LOOP ( 'NONE', ( #16487, #3089, #589, #10486 ) ) ;
#1100 = VECTOR ( 'NONE', #13955, 1000.000000000000000 ) ;
#1101 = VECTOR ( 'NONE', #12796, 1000.000000000000000 ) ;
#1102 = CARTESIAN_POINT ( 'NONE',  ( -0.5372984490435469551, 4.250000000000000000, 7.700000000000000178 ) ) ;
#1103 = CARTESIAN_POINT ( 'NONE',  ( 0.004026115436748929806, -0.3861894795279390280, 2.487698411375030005 ) ) ;
#1104 = VECTOR ( 'NONE', #14771, 1000.000000000000000 ) ;
#1105 = ADVANCED_FACE ( 'NONE', ( #1069 ), #9498, .F. ) ;
#1106 = VERTEX_POINT ( 'NONE', #8300 ) ;
#1107 = AXIS2_PLACEMENT_3D ( 'NONE', #16098, #3393, #13312 ) ;
#1108 = VECTOR ( 'NONE', #5713, 1000.000000000000000 ) ;
#1109 = CARTESIAN_POINT ( 'NONE',  ( 2.102728310581320148, -4.241953435693879726, 5.757014351541050345 ) ) ;
#1110 = ADVANCED_FACE ( 'NONE', ( #13938 ), #2743, .F. ) ;
#1111 = CARTESIAN_POINT ( 'NONE',  ( -0.4360591020458099987, -5.591101694915249887, 2.387347919655840034 ) ) ;
#1112 = EDGE_CURVE ( 'NONE', #2205, #3830, #18076, .T. ) ;
#1113 = CARTESIAN_POINT ( 'NONE',  ( -1.000000000000000000, -7.000000000000000000, 3.700000000000000178 ) ) ;
#1114 = EDGE_CURVE ( 'NONE', #7267, #17532, #1440, .T. ) ;
#1115 = CARTESIAN_POINT ( 'NONE',  ( 3.673940397442067510E-17, 3.581751045813930112, 7.750000000000000000 ) ) ;
#1116 = VECTOR ( 'NONE', #14485, 1000.000000000000000 ) ;
#1117 = CARTESIAN_POINT ( 'NONE',  ( 1.687170344132030042, -2.751502985243429844, 6.340793075730549511 ) ) ;
#1118 = CIRCLE ( 'NONE', #2598, 0.1000000000000000472 ) ;
#1119 = CARTESIAN_POINT ( 'NONE',  ( -1.722199153441400066, -5.095857339597789526, 3.099360556065549943 ) ) ;
#1120 = CARTESIAN_POINT ( 'NONE',  ( -1.520647680314179517, -1.959701183441630024, 3.320676805464663151 ) ) ;
#1121 = CARTESIAN_POINT ( 'NONE',  ( 1.899999999999999911, 6.661338147750959950E-17, 9.441371669411539713 ) ) ;
#1122 = AXIS2_PLACEMENT_3D ( 'NONE', #9742, #8440, #15576 ) ;
#1123 = CARTESIAN_POINT ( 'NONE',  ( -1.217041937262000051, -0.2742238837839079402, 2.666998181419179659 ) ) ;
#1124 = EDGE_LOOP ( 'NONE', ( #2346, #17137, #10697, #13392 ) ) ;
#1125 = AXIS2_PLACEMENT_3D ( 'NONE', #14643, #13263, #18230 ) ;
#1126 = CARTESIAN_POINT ( 'NONE',  ( 0.5999999999999999778, 0.5999999999999999778, 7.599999999999999645 ) ) ;
#1127 = PLANE ( 'NONE',  #6263 ) ;
#1128 = ORIENTED_EDGE ( 'NONE', *, *, #11746, .F. ) ;
#1129 = ORIENTED_EDGE ( 'NONE', *, *, #6937, .F. ) ;
#1130 = AXIS2_PLACEMENT_3D ( 'NONE', #4959, #6256, #13588 ) ;
#1131 = ORIENTED_EDGE ( 'NONE', *, *, #379, .F. ) ;
#1132 = LINE ( 'NONE', #1040, #10906 ) ;
#1133 = CARTESIAN_POINT ( 'NONE',  ( 1.562863241354470523, -5.108686440677975504, 6.031217337312382298 ) ) ;
#1134 = ADVANCED_FACE ( 'NONE', ( #1339 ), #56, .F. ) ;
#1135 = DIRECTION ( 'NONE',  ( -1.000000000000000000, 0.000000000000000000, 0.000000000000000000 ) ) ;
#1136 = VECTOR ( 'NONE', #10624, 1000.000000000000000 ) ;
#1137 = CARTESIAN_POINT ( 'NONE',  ( -1.250000000000000000, 3.500000000000000000, 5.100000000000000533 ) ) ;
#1138 = CARTESIAN_POINT ( 'NONE',  ( -2.185196738168510233, -4.758136654396205145, 3.194002352996703653 ) ) ;
#1139 = VECTOR ( 'NONE', #16114, 1000.000000000000000 ) ;
#1140 = LINE ( 'NONE', #13645, #6405 ) ;
#1141 = CARTESIAN_POINT ( 'NONE',  ( -2.267872052190610166, -1.843259742000189938, 4.071110468860649867 ) ) ;
#1142 = CARTESIAN_POINT ( 'NONE',  ( -0.7998959936908373036, -0.1646186440677970542, 7.230419212249866945 ) ) ;
#1143 = VECTOR ( 'NONE', #11238, 1000.000000000000000 ) ;
#1144 = CARTESIAN_POINT ( 'NONE',  ( 1.378221871957440170, -0.4201271186440679872, 6.607619368096269596 ) ) ;
#1145 = EDGE_LOOP ( 'NONE', ( #14306, #2927, #14326, #11786 ) ) ;
#1146 = CARTESIAN_POINT ( 'NONE',  ( -0.07064654565474801085, -0.1512711864406789675, 7.352897294663512717 ) ) ;
#1147 = ORIENTED_EDGE ( 'NONE', *, *, #10999, .T. ) ;
#1148 = MECHANICAL_DESIGN_GEOMETRIC_PRESENTATION_REPRESENTATION (  '', ( #6157 ), #4396 ) ;
#1149 = CARTESIAN_POINT ( 'NONE',  ( -1.899999999999999911, 2.000000000000000000, 2.388061258337340122E-16 ) ) ;
#1150 = CARTESIAN_POINT ( 'NONE',  ( -0.9719602541832296216, -2.755343861603410271, 6.843370931913549171 ) ) ;
#1151 = DIRECTION ( 'NONE',  ( 0.000000000000000000, 0.000000000000000000, 1.000000000000000000 ) ) ;
#1152 = CARTESIAN_POINT ( 'NONE',  ( -2.345900685764729765, -5.528813559322030002, 4.512231114381339836 ) ) ;
#1153 = CARTESIAN_POINT ( 'NONE',  ( -2.589817782457070727, -4.963890372630814340, 4.120381550730010112 ) ) ;
#1154 = EDGE_CURVE ( 'NONE', #16167, #11049, #10982, .T. ) ;
#1155 = ORIENTED_EDGE ( 'NONE', *, *, #1986, .T. ) ;
#1156 = CARTESIAN_POINT ( 'NONE',  ( -1.294880990849879732, -4.829629811528119987, 3.097365952343163364 ) ) ;
#1157 = CARTESIAN_POINT ( 'NONE',  ( -1.704669856830349994, -4.796950468210010143, 3.080704711052660194 ) ) ;
#1158 = CARTESIAN_POINT ( 'NONE',  ( 0.6919952253610313075, -4.451548030288480895, 7.262080463427998289 ) ) ;
#1159 = CARTESIAN_POINT ( 'NONE',  ( 0.4000000000000000222, -1.399999999999999911, 5.100000000000000533 ) ) ;
#1160 = DIRECTION ( 'NONE',  ( -1.000000000000000000, 0.000000000000000000, 0.000000000000000000 ) ) ;
#1161 = DIRECTION ( 'NONE',  ( 2.220446049250319983E-16, 0.000000000000000000, 1.000000000000000000 ) ) ;
#1162 = AXIS2_PLACEMENT_3D ( 'NONE', #13573, #887, #8023 ) ;
#1163 = CARTESIAN_POINT ( 'NONE',  ( 1.436030008293490701, -1.191187669928120529, 6.167214932417436124 ) ) ;
#1164 = PLANE ( 'NONE',  #16782 ) ;
#1165 = ORIENTED_EDGE ( 'NONE', *, *, #5182, .F. ) ;
#1166 = DIRECTION ( 'NONE',  ( 0.000000000000000000, -1.000000000000000000, -8.934339325041029556E-19 ) ) ;
#1167 = PLANE ( 'NONE',  #5570 ) ;
#1168 = CARTESIAN_POINT ( 'NONE',  ( 0.7476103186298468373, -0.3177966101694921219, 2.787995836256459636 ) ) ;
#1169 = CARTESIAN_POINT ( 'NONE',  ( 2.049607015837390911, -2.429307825567371459, 6.385889905549011480 ) ) ;
#1170 = FACE_OUTER_BOUND ( 'NONE', #7408, .T. ) ;
#1171 = CARTESIAN_POINT ( 'NONE',  ( -0.9138909625329535436, -4.911779243796845051, 2.204775695797560164 ) ) ;
#1172 = CARTESIAN_POINT ( 'NONE',  ( -0.1365430262726299304, -5.153177966101685215, 6.748423079423377047 ) ) ;
#1173 = VERTEX_POINT ( 'NONE', #3930 ) ;
#1174 = DIRECTION ( 'NONE',  ( -0.7071067811865475727, -4.040679121612663150E-17, -0.7071067811865475727 ) ) ;
#1175 = LINE ( 'NONE', #2754, #17388 ) ;
#1176 = VECTOR ( 'NONE', #7596, 1000.000000000000000 ) ;
#1177 = LINE ( 'NONE', #9309, #793 ) ;
#1178 = VERTEX_POINT ( 'NONE', #9583 ) ;
#1179 = CARTESIAN_POINT ( 'NONE',  ( -1.378221871957430178, -5.479872881355929870, 6.607619368096279366 ) ) ;
#1180 = CARTESIAN_POINT ( 'NONE',  ( 2.461935615161780611, -3.919758276017824006, 5.690952430644305338 ) ) ;
#1181 = CARTESIAN_POINT ( 'NONE',  ( 2.607432201095279733, -4.078935417675873865, 4.205620581240154365 ) ) ;
#1182 = DIRECTION ( 'NONE',  ( 1.000000000000000000, 0.000000000000000000, 0.000000000000000000 ) ) ;
#1183 = CARTESIAN_POINT ( 'NONE',  ( 1.990095963740240004, -0.7525510688106187285, 5.204400533041760646 ) ) ;
#1184 = DIRECTION ( 'NONE',  ( 7.930164461608269807E-17, 0.000000000000000000, 1.000000000000000000 ) ) ;
#1185 = ORIENTED_EDGE ( 'NONE', *, *, #13562, .T. ) ;
#1186 = CIRCLE ( 'NONE', #12134, 0.1499999999999999667 ) ;
#1187 = CARTESIAN_POINT ( 'NONE',  ( -0.9000000000000000222, 6.450000000000000178, 1.600000000000000089 ) ) ;
#1188 = CARTESIAN_POINT ( 'NONE',  ( 1.549742865090599997, -0.4156779661016959948, 6.471102547561449647 ) ) ;
#1189 = CARTESIAN_POINT ( 'NONE',  ( 1.991984774470479946, -3.985782264522710339, 3.446707398186009907 ) ) ;
#1190 = CARTESIAN_POINT ( 'NONE',  ( 1.899999999999999911, 2.000000000000000000, 1.600000000000000089 ) ) ;
#1191 = CARTESIAN_POINT ( 'NONE',  ( 2.500000000000000000, 0.4000000000000000222, 4.000000000000000000 ) ) ;
#1192 = CARTESIAN_POINT ( 'NONE',  ( -2.645377369053839356, -5.528813559322025561, 4.488260618344918740 ) ) ;
#1193 = EDGE_LOOP ( 'NONE', ( #13437, #4135, #9475 ) ) ;
#1194 = LINE ( 'NONE', #10731, #16399 ) ;
#1195 = VERTEX_POINT ( 'NONE', #15243 ) ;
#1196 = CARTESIAN_POINT ( 'NONE',  ( -2.306642602145299925, -5.215466101694908652, 5.166805192608489250 ) ) ;
#1197 = FACE_OUTER_BOUND ( 'NONE', #10533, .T. ) ;
#1198 = CARTESIAN_POINT ( 'NONE',  ( -0.2335786437626909962, 6.450000000000000178, 2.241421356237310203 ) ) ;
#1199 = ORIENTED_EDGE ( 'NONE', *, *, #2728, .T. ) ;
#1200 = VECTOR ( 'NONE', #13384, 1000.000000000000000 ) ;
#1201 = CARTESIAN_POINT ( 'NONE',  ( 1.724579595320000047, -3.939205687946140344, 3.098572228637889836 ) ) ;
#1202 =( NAMED_UNIT ( * ) SI_UNIT ( $, .STERADIAN. ) SOLID_ANGLE_UNIT ( ) );
#1203 = CARTESIAN_POINT ( 'NONE',  ( 0.5070585469427659753, -5.011796459788054214, 2.696565570857651473 ) ) ;
#1204 = CARTESIAN_POINT ( 'NONE',  ( 1.800000000000000044, 0.5999999999999999778, 1.600000000000000089 ) ) ;
#1205 = DIRECTION ( 'NONE',  ( -1.000000000000000000, 0.000000000000000000, 0.000000000000000000 ) ) ;
#1206 = CARTESIAN_POINT ( 'NONE',  ( -2.036228139452650243, -3.473439922180369788, 3.519948877554409883 ) ) ;
#1207 = DIRECTION ( 'NONE',  ( -1.216682766712499758E-16, 6.416248801027068947E-32, -1.000000000000000000 ) ) ;
#1208 = CARTESIAN_POINT ( 'NONE',  ( -1.423520578776781509, -3.543304787045241433, 3.220645071516951230 ) ) ;
#1209 = CARTESIAN_POINT ( 'NONE',  ( 1.899999999999999911, 2.799999999999999822, 1.600000000000000089 ) ) ;
#1210 = AXIS2_PLACEMENT_3D ( 'NONE', #1745, #15811, #1911 ) ;
#1211 = CARTESIAN_POINT ( 'NONE',  ( -0.3897427956305680175, -0.2909039927201511055, 2.676097687607990938 ) ) ;
#1212 = ORIENTED_EDGE ( 'NONE', *, *, #177, .F. ) ;
#1213 = ADVANCED_FACE ( 'NONE', ( #2544 ), #12549, .T. ) ;
#1214 = EDGE_LOOP ( 'NONE', ( #9557, #9004, #14417, #13828 ) ) ;
#1215 = ADVANCED_FACE ( 'NONE', ( #12637 ), #18262, .T. ) ;
#1216 = EDGE_LOOP ( 'NONE', ( #18170, #9335, #81, #3535 ) ) ;
#1217 = VECTOR ( 'NONE', #5462, 1000.000000000000000 ) ;
#1218 = PRODUCT_DEFINITION_CONTEXT ( 'detailed design', #244, 'design' ) ;
#1219 = EDGE_LOOP ( 'NONE', ( #14780, #16677, #16057, #10611 ) ) ;
#1220 = LINE ( 'NONE', #6866, #7945 ) ;
#1221 = CARTESIAN_POINT ( 'NONE',  ( 1.679950111053631900, -5.104237288135595740, 5.880020650119711867 ) ) ;
#1222 = PRODUCT_DEFINITION_SHAPE ( 'NONE', 'NONE',  #7122 ) ;
#1223 = CARTESIAN_POINT ( 'NONE',  ( 0.7785957873161482024, -1.940253771513320125, 2.162894899107371316 ) ) ;
#1224 = LINE ( 'NONE', #9917, #13232 ) ;
#1225 = CARTESIAN_POINT ( 'NONE',  ( -1.500000000000000000, -5.599999999999999645, 2.299999999999999822 ) ) ;
#1226 = PLANE ( 'NONE',  #11118 ) ;
#1227 = CARTESIAN_POINT ( 'NONE',  ( -0.8298945877350979439, -5.211074464177370302, 2.494426474263899962 ) ) ;
#1228 = DIRECTION ( 'NONE',  ( 0.000000000000000000, -0.2588190451025150218, 0.9659258262890698665 ) ) ;
#1229 = CARTESIAN_POINT ( 'NONE',  ( -2.353343516942199898, -1.773394877135329839, 4.722803042560189901 ) ) ;
#1230 = CARTESIAN_POINT ( 'NONE',  ( -2.625437065641401446, -0.2180084745762719822, 5.087214675345155257 ) ) ;
#1231 = ADVANCED_FACE ( 'NONE', ( #13005 ), #4294, .T. ) ;
#1232 = ORIENTED_EDGE ( 'NONE', *, *, #3465, .T. ) ;
#1233 = CARTESIAN_POINT ( 'NONE',  ( 1.889104232906359870, -0.3444915254237289615, 3.296507079072520163 ) ) ;
#1234 = CARTESIAN_POINT ( 'NONE',  ( -1.300961508564169922, -0.4779661016949160457, 6.661123742937279602 ) ) ;
#1235 = VERTEX_POINT ( 'NONE', #14301 ) ;
#1236 = EDGE_CURVE ( 'NONE', #9612, #14617, #12910, .T. ) ;
#1237 = CARTESIAN_POINT ( 'NONE',  ( -1.661700935788390066, -0.2625000000000000111, 3.038299064211610112 ) ) ;
#1238 = CARTESIAN_POINT ( 'NONE',  ( 2.291237445532070094, -0.9350164987569499209, 4.162434510291790346 ) ) ;
#1239 = ORIENTED_EDGE ( 'NONE', *, *, #17143, .T. ) ;
#1240 = EDGE_CURVE ( 'NONE', #15103, #7787, #232, .T. ) ;
#1241 = CARTESIAN_POINT ( 'NONE',  ( -1.899999999999999911, 7.299999999999999822, 1.600000000000000089 ) ) ;
#1242 = CARTESIAN_POINT ( 'NONE',  ( 0.3159454637157338985, -2.615614131873679415, 7.032150113402087399 ) ) ;
#1243 =( LENGTH_UNIT ( ) NAMED_UNIT ( * ) SI_UNIT ( .MILLI., .METRE. ) );
#1244 = CARTESIAN_POINT ( 'NONE',  ( 1.254903241568450900, -5.426483050847465073, 7.038391080368498365 ) ) ;
#1245 = ORIENTED_EDGE ( 'NONE', *, *, #7119, .T. ) ;
#1246 = CARTESIAN_POINT ( 'NONE',  ( 1.928817277882869829, -1.144611093351550091, 6.048484184565929844 ) ) ;
#1247 = CARTESIAN_POINT ( 'NONE',  ( -0.06276132972181580616, -4.222506023765570049, 7.052616990284530374 ) ) ;
#1248 = ORIENTED_EDGE ( 'NONE', *, *, #10846, .F. ) ;
#1249 = DIRECTION ( 'NONE',  ( 3.018987445473099952E-48, 1.000000000000000000, 2.465190328815659976E-32 ) ) ;
#1250 = DIRECTION ( 'NONE',  ( -5.551115123125880521E-15, 1.000000000000000000, 6.055990775824630636E-30 ) ) ;
#1251 = DIRECTION ( 'NONE',  ( 0.7071067811865470176, -5.772398745161022854E-18, 0.7071067811865480168 ) ) ;
#1252 = CARTESIAN_POINT ( 'NONE',  ( 1.485933537025759366, -0.8030495317899833951, 3.286232459959989249 ) ) ;
#1253 = EDGE_LOOP ( 'NONE', ( #13255, #13253, #16458, #2501, #11937, #987, #6096, #17907, #4300, #6844, #7260, #3756, #14489, #3680 ) ) ;
#1254 = DIRECTION ( 'NONE',  ( 1.224646799147350002E-16, 1.000000000000000000, 1.059261469412979938E-31 ) ) ;
#1255 = CARTESIAN_POINT ( 'NONE',  ( -0.1749999999999999889, 9.299999999999998934, 1.600000000000000089 ) ) ;
#1256 = CARTESIAN_POINT ( 'NONE',  ( 0.9222751404130974384, -0.3222457627118649470, 2.865854510788131027 ) ) ;
#1257 = AXIS2_PLACEMENT_3D ( 'NONE', #1204, #11100, #6852 ) ;
#1258 = EDGE_CURVE ( 'NONE', #16824, #6139, #11523, .T. ) ;
#1259 = CARTESIAN_POINT ( 'NONE',  ( -2.022685914314908739, -4.432100618360157007, 6.418096442297106741 ) ) ;
#1260 = CARTESIAN_POINT ( 'NONE',  ( -0.1881942810071039751, -5.280843314568230085, 2.350674491507239949 ) ) ;
#1261 = CARTESIAN_POINT ( 'NONE',  ( -0.7476103186298618253, -5.282203389830510076, 2.787995836256459636 ) ) ;
#1262 = EDGE_LOOP ( 'NONE', ( #7154, #5175, #6966, #5110 ) ) ;
#1263 = CARTESIAN_POINT ( 'NONE',  ( 1.707817112497189704, -0.1112288135593230004, 6.319218296629480314 ) ) ;
#1264 = DIRECTION ( 'NONE',  ( 0.000000000000000000, -1.000000000000000000, 0.000000000000000000 ) ) ;
#1265 = DIRECTION ( 'NONE',  ( 0.000000000000000000, 0.000000000000000000, -1.000000000000000000 ) ) ;
#1266 = EDGE_CURVE ( 'NONE', #8350, #17672, #4473, .T. ) ;
#1267 = ORIENTED_EDGE ( 'NONE', *, *, #15981, .T. ) ;
#1268 = CARTESIAN_POINT ( 'NONE',  ( -0.4360591020458099987, -5.591101694915249887, 2.387347919655840034 ) ) ;
#1269 = CARTESIAN_POINT ( 'NONE',  ( -2.584100759211431786, -4.664983501243040287, 4.095403473953163953 ) ) ;
#1270 = CARTESIAN_POINT ( 'NONE',  ( 2.549960444629811640, -4.055647129387581984, 3.964598460822105874 ) ) ;
#1271 = EDGE_CURVE ( 'NONE', #17781, #8865, #17065, .T. ) ;
#1272 = CARTESIAN_POINT ( 'NONE',  ( 1.800000000000000044, 7.799999999999999822, 7.599999999999999645 ) ) ;
#1273 = DIRECTION ( 'NONE',  ( -1.000000000000000000, 0.000000000000000000, 0.000000000000000000 ) ) ;
#1274 = VECTOR ( 'NONE', #1642, 1000.000000000000000 ) ;
#1275 = EDGE_LOOP ( 'NONE', ( #4293, #12382, #1615, #14286 ) ) ;
#1276 = EDGE_CURVE ( 'NONE', #3896, #1735, #15705, .T. ) ;
#1277 = DIRECTION ( 'NONE',  ( 1.000000000000000000, 0.000000000000000000, 6.344131569286600069E-16 ) ) ;
#1278 = CARTESIAN_POINT ( 'NONE',  ( 0.2469343877495150108, -0.3044491525423730915, 2.057675570509529539 ) ) ;
#1279 = CARTESIAN_POINT ( 'NONE',  ( -2.159566522375440112, -3.240557039297490061, 5.635424033751089468 ) ) ;
#1280 = FACE_OUTER_BOUND ( 'NONE', #5828, .T. ) ;
#1281 = DIRECTION ( 'NONE',  ( -1.000000000000000000, 0.000000000000000000, 0.000000000000000000 ) ) ;
#1282 = CARTESIAN_POINT ( 'NONE',  ( 2.630358833876468960, -5.068644067796615360, 4.347767980622404771 ) ) ;
#1283 = ORIENTED_EDGE ( 'NONE', *, *, #4749, .F. ) ;
#1284 = ORIENTED_EDGE ( 'NONE', *, *, #16946, .F. ) ;
#1285 = CARTESIAN_POINT ( 'NONE',  ( -3.760880495917719358E-15, -5.299999999999999822, 2.350000000000000089 ) ) ;
#1286 = FACE_OUTER_BOUND ( 'NONE', #14909, .T. ) ;
#1287 = FACE_OUTER_BOUND ( 'NONE', #9651, .T. ) ;
#1288 = ORIENTED_EDGE ( 'NONE', *, *, #2367, .T. ) ;
#1289 = CARTESIAN_POINT ( 'NONE',  ( -2.283153923255329953, -3.403575057315510133, 4.129076318403500423 ) ) ;
#1290 = LINE ( 'NONE', #13886, #16791 ) ;
#1291 = CARTESIAN_POINT ( 'NONE',  ( 0.8611469534735395337, -5.020626044399135068, 2.833474624362548600 ) ) ;
#1292 = DIRECTION ( 'NONE',  ( -1.000000000000000000, 0.000000000000000000, 0.000000000000000000 ) ) ;
#1293 = DIRECTION ( 'NONE',  ( -0.7071067811865475727, -4.617918996128746176E-17, -0.7071067811865475727 ) ) ;
#1294 = CARTESIAN_POINT ( 'NONE',  ( -1.092567884283820012, -4.637854336594780413, 6.784476218553590066 ) ) ;
#1295 = PLANE ( 'NONE',  #13490 ) ;
#1296 = CARTESIAN_POINT ( 'NONE',  ( 1.627161714697888728, -3.962493976234419790, 3.448102801005814122 ) ) ;
#1297 = LINE ( 'NONE', #2509, #9090 ) ;
#1298 = VERTEX_POINT ( 'NONE', #1624 ) ;
#1299 = CARTESIAN_POINT ( 'NONE',  ( 0.5000000000000000000, 5.762741699796949391, 5.100000000000000533 ) ) ;
#1300 = VERTEX_POINT ( 'NONE', #7364 ) ;
#1301 = ORIENTED_EDGE ( 'NONE', *, *, #4407, .T. ) ;
#1302 = ORIENTED_EDGE ( 'NONE', *, *, #9005, .T. ) ;
#1303 = ADVANCED_FACE ( 'NONE', ( #327 ), #11605, .F. ) ;
#1304 = ORIENTED_EDGE ( 'NONE', *, *, #17396, .F. ) ;
#1305 = DIRECTION ( 'NONE',  ( -1.746418240983389920E-16, 1.000000000000000000, 0.000000000000000000 ) ) ;
#1306 = CARTESIAN_POINT ( 'NONE',  ( 1.289141334274990447, -5.117584745762705722, 6.297747079672416426 ) ) ;
#1307 = DIRECTION ( 'NONE',  ( 0.000000000000000000, -1.000000000000000000, 1.850371707708589879E-16 ) ) ;
#1308 = LINE ( 'NONE', #8629, #11152 ) ;
#1309 = LINE ( 'NONE', #8358, #17308 ) ;
#1310 = DIRECTION ( 'NONE',  ( -2.055968564120659776E-16, -1.000000000000000000, 0.000000000000000000 ) ) ;
#1311 = CARTESIAN_POINT ( 'NONE',  ( -0.1749999999999999889, 7.700000000000000178, 1.600000000000000089 ) ) ;
#1312 = ADVANCED_FACE ( 'NONE', ( #17507 ), #4030, .T. ) ;
#1313 = CARTESIAN_POINT ( 'NONE',  ( 2.331386066015260106, -0.9583047870452390260, 4.378465089518139841 ) ) ;
#1314 = CARTESIAN_POINT ( 'NONE',  ( 0.2739924515130530702, -2.615614131873680748, 6.734657214162127481 ) ) ;
#1315 = CARTESIAN_POINT ( 'NONE',  ( 1.088937603231269646, -0.02669491525423760975, 2.959627624143540192 ) ) ;
#1316 = EDGE_LOOP ( 'NONE', ( #3594, #10951, #16968, #14515 ) ) ;
#1317 = CARTESIAN_POINT ( 'NONE',  ( -2.293398556041709835, -0.5358050847457630494, 4.171956209133480975 ) ) ;
#1318 = CARTESIAN_POINT ( 'NONE',  ( 1.800000000000000044, 11.40000000000000036, 6.599999999999999645 ) ) ;
#1319 = ORIENTED_EDGE ( 'NONE', *, *, #11624, .T. ) ;
#1320 = CARTESIAN_POINT ( 'NONE',  ( 1.549742865090599997, -0.1156779661016950067, 6.471102547561449647 ) ) ;
#1321 = CARTESIAN_POINT ( 'NONE',  ( 0.1749999999999999889, 2.700000000000000178, 0.5999999999999999778 ) ) ;
#1322 = ORIENTED_EDGE ( 'NONE', *, *, #14561, .F. ) ;
#1323 = FACE_OUTER_BOUND ( 'NONE', #12895, .T. ) ;
#1324 = ORIENTED_EDGE ( 'NONE', *, *, #3238, .F. ) ;
#1325 = CARTESIAN_POINT ( 'NONE',  ( 2.137408332595948757, -2.149848366107911080, 3.714996798363940922 ) ) ;
#1326 = CARTESIAN_POINT ( 'NONE',  ( 2.191755591049679541, -5.346398305084745672, 3.203650300307709475 ) ) ;
#1327 = ORIENTED_EDGE ( 'NONE', *, *, #6740, .F. ) ;
#1328 = EDGE_CURVE ( 'NONE', #14407, #3917, #8228, .T. ) ;
#1329 = DIRECTION ( 'NONE',  ( 1.000000000000000000, 0.000000000000000000, 0.000000000000000000 ) ) ;
#1330 = CARTESIAN_POINT ( 'NONE',  ( -0.4339619423229766348, -0.4601694915254239682, 6.706578715862737461 ) ) ;
#1331 = VERTEX_POINT ( 'NONE', #15270 ) ;
#1332 = EDGE_CURVE ( 'NONE', #2090, #7773, #3777, .T. ) ;
#1333 = DIRECTION ( 'NONE',  ( -6.167905692361979821E-17, 0.000000000000000000, -1.000000000000000000 ) ) ;
#1334 = CARTESIAN_POINT ( 'NONE',  ( -1.889999999999999902, 7.299999999999999822, 0.5999999999999999778 ) ) ;
#1335 = EDGE_CURVE ( 'NONE', #7787, #10555, #11657, .T. ) ;
#1336 = CARTESIAN_POINT ( 'NONE',  ( 1.440522616026430391, -0.7952867690272208412, 3.241384813161591438 ) ) ;
#1337 = DIRECTION ( 'NONE',  ( 7.401486830834380223E-16, 1.000000000000000000, -1.110223024625159992E-16 ) ) ;
#1338 = ORIENTED_EDGE ( 'NONE', *, *, #7317, .T. ) ;
#1339 = FACE_OUTER_BOUND ( 'NONE', #6141, .T. ) ;
#1340 = CARTESIAN_POINT ( 'NONE',  ( 4.898587196589409994E-17, 0.1000000000000000056, 7.700000000000000178 ) ) ;
#1341 = CARTESIAN_POINT ( 'NONE',  ( 2.653777292528160192, -3.826605122864674247, 4.724078510415155030 ) ) ;
#1342 = VECTOR ( 'NONE', #8161, 1000.000000000000000 ) ;
#1343 = ORIENTED_EDGE ( 'NONE', *, *, #15845, .T. ) ;
#1344 = CARTESIAN_POINT ( 'NONE',  ( 0.5000000000000000000, 3.500000000000000000, 5.100000000000000533 ) ) ;
#1345 = CARTESIAN_POINT ( 'NONE',  ( -1.042222075699109407, -5.175423728813555613, 6.468743694056166227 ) ) ;
#1346 = ORIENTED_EDGE ( 'NONE', *, *, #6220, .T. ) ;
#1347 = CIRCLE ( 'NONE', #10824, 0.5500000000000001554 ) ;
#1348 = PLANE ( 'NONE',  #12446 ) ;
#1349 = CARTESIAN_POINT ( 'NONE',  ( 1.000000000000000000, -5.000000000000000000, 6.100000000000000533 ) ) ;
#1350 = DIRECTION ( 'NONE',  ( -0.000000000000000000, 1.000000000000000000, 0.000000000000000000 ) ) ;
#1351 = EDGE_LOOP ( 'NONE', ( #12487, #10039, #8460, #3936 ) ) ;
#1352 = LINE ( 'NONE', #11168, #11141 ) ;
#1353 = CARTESIAN_POINT ( 'NONE',  ( -2.192143888961709752, -1.381334852594400031, 5.556300681753639559 ) ) ;
#1354 = EDGE_CURVE ( 'NONE', #11698, #14775, #3873, .T. ) ;
#1355 = CARTESIAN_POINT ( 'NONE',  ( 0.5500000000000000444, 6.450000000000000178, 3.200000000000000178 ) ) ;
#1356 = CARTESIAN_POINT ( 'NONE',  ( 1.703239418290648732, -0.5429564742160235546, 3.553755118148703929 ) ) ;
#1357 = CIRCLE ( 'NONE', #17589, 0.1499999999999999667 ) ;
#1358 = DIRECTION ( 'NONE',  ( 0.000000000000000000, -1.000000000000000000, 0.000000000000000000 ) ) ;
#1359 = EDGE_LOOP ( 'NONE', ( #549, #15650, #7823, #5403 ) ) ;
#1360 = DIRECTION ( 'NONE',  ( -6.938893903907229610E-17, 0.000000000000000000, -1.000000000000000000 ) ) ;
#1361 = CARTESIAN_POINT ( 'NONE',  ( -0.2812789908084309953, -0.4557203389830509765, 7.036533610117280624 ) ) ;
#1362 = CARTESIAN_POINT ( 'NONE',  ( 1.687170344132030042, -2.751502985243429844, 6.340793075730549511 ) ) ;
#1363 = DIRECTION ( 'NONE',  ( 2.220446049250309876E-16, -1.000000000000000000, 0.000000000000000000 ) ) ;
#1364 = CARTESIAN_POINT ( 'NONE',  ( 2.304156201936080617, -5.099788135593215976, 6.016707707703351282 ) ) ;
#1365 = ORIENTED_EDGE ( 'NONE', *, *, #5653, .F. ) ;
#1366 = PRODUCT_DEFINITION_SHAPE ( 'NONE', 'NONE',  #3578 ) ;
#1367 = VERTEX_POINT ( 'NONE', #5164 ) ;
#1368 = DIRECTION ( 'NONE',  ( 0.000000000000000000, 0.000000000000000000, -1.000000000000000000 ) ) ;
#1369 = LINE ( 'NONE', #7032, #17082 ) ;
#1370 = VECTOR ( 'NONE', #15490, 1000.000000000000000 ) ;
#1371 = VERTEX_POINT ( 'NONE', #2492 ) ;
#1372 = VECTOR ( 'NONE', #16701, 1000.000000000000000 ) ;
#1373 = CARTESIAN_POINT ( 'NONE',  ( 0.5606293434988925961, -1.330917399657850497, 7.293994686233932434 ) ) ;
#1374 = EDGE_CURVE ( 'NONE', #9933, #5569, #12126, .T. ) ;
#1375 = FILL_AREA_STYLE_COLOUR ( '', #2318 ) ;
#1376 = CARTESIAN_POINT ( 'NONE',  ( -1.699999999999999956, 2.299999999999999822, 7.599999999999999645 ) ) ;
#1377 = FACE_OUTER_BOUND ( 'NONE', #4552, .T. ) ;
#1378 = CARTESIAN_POINT ( 'NONE',  ( 0.6207106781186539912, 6.450000000000000178, 2.628553390593269423 ) ) ;
#1379 = CARTESIAN_POINT ( 'NONE',  ( -1.465095039565370127, -3.566593075333519991, 2.858195935359880480 ) ) ;
#1380 = SPHERICAL_SURFACE ( 'NONE', #5204, 0.2000000000000000111 ) ;
#1381 = CARTESIAN_POINT ( 'NONE',  ( 1.971820545011360171, -4.055647129387581984, 4.128313389260194199 ) ) ;
#1382 = AXIS2_PLACEMENT_3D ( 'NONE', #5481, #2799, #16771 ) ;
#1383 = CARTESIAN_POINT ( 'NONE',  ( -1.899999999999999911, 11.15000000000000036, 7.990820364436479856E-16 ) ) ;
#1384 = CIRCLE ( 'NONE', #8783, 1.016666666666670160 ) ;
#1385 = DIRECTION ( 'NONE',  ( 0.000000000000000000, -1.000000000000000000, 9.251858538542969116E-17 ) ) ;
#1386 = VECTOR ( 'NONE', #9240, 1000.000000000000000 ) ;
#1387 = ORIENTED_EDGE ( 'NONE', *, *, #18174, .F. ) ;
#1388 = CARTESIAN_POINT ( 'NONE',  ( -1.661700935788390066, -0.5625000000000000000, 3.038299064211610112 ) ) ;
#1389 = VERTEX_POINT ( 'NONE', #15100 ) ;
#1390 = FACE_OUTER_BOUND ( 'NONE', #7177, .T. ) ;
#1391 = ORIENTED_EDGE ( 'NONE', *, *, #8241, .T. ) ;
#1392 = CARTESIAN_POINT ( 'NONE',  ( 0.9000000000000000222, 2.050000000000000266, 3.600000000000000089 ) ) ;
#1393 = CIRCLE ( 'NONE', #11792, 0.5999999999999998668 ) ;
#1394 = FACE_OUTER_BOUND ( 'NONE', #824, .T. ) ;
#1395 = AXIS2_PLACEMENT_3D ( 'NONE', #3308, #1912, #6175 ) ;
#1396 = PRODUCT_DEFINITION_CONTEXT ( 'detailed design', #6861, 'design' ) ;
#1397 = EDGE_LOOP ( 'NONE', ( #10356, #9287, #15350, #6015 ) ) ;
#1398 = CARTESIAN_POINT ( 'NONE',  ( 2.050059171113549183, -5.077542372881359789, 4.809263467226075228 ) ) ;
#1399 = CARTESIAN_POINT ( 'NONE',  ( 0.04661003995938393929, -1.870388906648449812, 2.046522810126899294 ) ) ;
#1400 = AXIS2_PLACEMENT_3D ( 'NONE', #14762, #10784, #13285 ) ;
#1401 = CARTESIAN_POINT ( 'NONE',  ( -1.300000000000000044, 0.000000000000000000, 7.599999999999999645 ) ) ;
#1402 = CIRCLE ( 'NONE', #3436, 0.2000000000000000389 ) ;
#1403 = CARTESIAN_POINT ( 'NONE',  ( -0.1749999999999999889, 8.200000000000001066, 0.4000000000000000222 ) ) ;
#1404 = CARTESIAN_POINT ( 'NONE',  ( 1.875000000000000000, 12.00000000000000000, 7.700000000000000178 ) ) ;
#1405 = VECTOR ( 'NONE', #14615, 1000.000000000000000 ) ;
#1406 = CARTESIAN_POINT ( 'NONE',  ( -1.599999999999869971, 12.00000000000000000, -2.399999999999999911 ) ) ;
#1407 = CARTESIAN_POINT ( 'NONE',  ( -0.1749999999999999889, 9.500000000000000000, 1.600000000000000089 ) ) ;
#1408 = CARTESIAN_POINT ( 'NONE',  ( 0.7678268402137939930, -2.867944426684879922, 6.924676972266129660 ) ) ;
#1409 = VECTOR ( 'NONE', #12608, 1000.000000000000000 ) ;
#1410 = AXIS2_PLACEMENT_3D ( 'NONE', #9640, #2616, #2796 ) ;
#1411 = CARTESIAN_POINT ( 'NONE',  ( 1.238036348455360258, -3.593722239981790523, 3.062267469172269330 ) ) ;
#1412 = VECTOR ( 'NONE', #15765, 1000.000000000000000 ) ;
#1413 = CARTESIAN_POINT ( 'NONE',  ( 2.012177589105479392, -0.08453389830508521718, 5.107213040360584877 ) ) ;
#1414 = ORIENTED_EDGE ( 'NONE', *, *, #13897, .T. ) ;
#1415 = DIRECTION ( 'NONE',  ( 6.344131569286600069E-16, 1.000000000000000000, 1.586032892321649771E-16 ) ) ;
#1416 = CARTESIAN_POINT ( 'NONE',  ( 1.149999999999999911, 9.274118095489749081, 7.596592582628910684 ) ) ;
#1417 = ORIENTED_EDGE ( 'NONE', *, *, #7444, .F. ) ;
#1418 = AXIS2_PLACEMENT_3D ( 'NONE', #1340, #6991, #14219 ) ;
#1419 = CARTESIAN_POINT ( 'NONE',  ( -2.155845792290839835, -0.2447033898305089883, 3.756158857535780271 ) ) ;
#1420 = AXIS2_PLACEMENT_3D ( 'NONE', #911, #2006, #6550 ) ;
#1421 = CARTESIAN_POINT ( 'NONE',  ( 1.265407828724300021, -2.309025507765960050, 2.715689360385540319 ) ) ;
#1422 = ORIENTED_EDGE ( 'NONE', *, *, #12562, .F. ) ;
#1423 = FACE_OUTER_BOUND ( 'NONE', #2648, .T. ) ;
#1424 = ORIENTED_EDGE ( 'NONE', *, *, #1476, .T. ) ;
#1425 = CARTESIAN_POINT ( 'NONE',  ( 2.036228139452629371, -2.126560077819630301, 3.519948877554369915 ) ) ;
#1426 = SHAPE_REPRESENTATION_RELATIONSHIP ( 'NONE' , 'NONE' ,  #16004, #6205 ) ;
#1427 = CARTESIAN_POINT ( 'NONE',  ( 2.508228811380011081, -5.390889830508485581, 5.566973598334535644 ) ) ;
#1428 = VECTOR ( 'NONE', #3053, 1000.000000000000000 ) ;
#1429 = ORIENTED_EDGE ( 'NONE', *, *, #14388, .F. ) ;
#1430 = CARTESIAN_POINT ( 'NONE',  ( -1.699999999999999956, 2.299999999999999822, 7.599999999999999645 ) ) ;
#1431 = CARTESIAN_POINT ( 'NONE',  ( 0.2189795514005130062, -0.3044491525423729805, 2.356806637999009801 ) ) ;
#1432 = VERTEX_POINT ( 'NONE', #1190 ) ;
#1433 = VECTOR ( 'NONE', #2358, 1000.000000000000000 ) ;
#1434 = LINE ( 'NONE', #6706, #13508 ) ;
#1435 = DIRECTION ( 'NONE',  ( 1.000000000000000000, 0.000000000000000000, 0.000000000000000000 ) ) ;
#1436 = DIRECTION ( 'NONE',  ( -1.000000000000000000, 2.220446049250309876E-16, 0.000000000000000000 ) ) ;
#1437 = CARTESIAN_POINT ( 'NONE',  ( -1.583713126240711588, -3.170692174432623744, 6.006428174987420654 ) ) ;
#1438 = CARTESIAN_POINT ( 'NONE',  ( 1.899999999999999911, 12.00000000000000000, 7.649999999999999467 ) ) ;
#1439 = ORIENTED_EDGE ( 'NONE', *, *, #16868, .T. ) ;
#1440 = LINE ( 'NONE', #11254, #16332 ) ;
#1441 = VECTOR ( 'NONE', #15725, 1000.000000000000000 ) ;
#1442 = DIRECTION ( 'NONE',  ( 1.224646799147350002E-16, -1.000000000000000000, -6.123233995736769734E-17 ) ) ;
#1443 = VECTOR ( 'NONE', #1668, 1000.000000000000000 ) ;
#1444 = VECTOR ( 'NONE', #13642, 1000.000000000000000 ) ;
#1445 = ORIENTED_EDGE ( 'NONE', *, *, #14789, .F. ) ;
#1446 = CARTESIAN_POINT ( 'NONE',  ( 2.200000000000000178, 1.071498764318550058E-16, 4.000000000000000000 ) ) ;
#1447 = CARTESIAN_POINT ( 'NONE',  ( 1.661700935788380074, -5.337500000000000355, 3.038299064211610112 ) ) ;
#1448 = ORIENTED_EDGE ( 'NONE', *, *, #2634, .F. ) ;
#1449 = EDGE_CURVE ( 'NONE', #16145, #12528, #13775, .T. ) ;
#1450 = AXIS2_PLACEMENT_3D ( 'NONE', #13857, #4027, #12749 ) ;
#1451 = CARTESIAN_POINT ( 'NONE',  ( 0.6500000000000000222, 6.450000000000000178, 3.200000000000000178 ) ) ;
#1452 = ADVANCED_FACE ( 'NONE', ( #12397 ), #12483, .F. ) ;
#1453 = DIRECTION ( 'NONE',  ( -2.960594732333750117E-16, -1.000000000000000000, 0.000000000000000000 ) ) ;
#1454 = FACE_OUTER_BOUND ( 'NONE', #9654, .T. ) ;
#1455 = EDGE_CURVE ( 'NONE', #6816, #5243, #6923, .T. ) ;
#1456 = EDGE_LOOP ( 'NONE', ( #16915, #13820, #14175, #17317 ) ) ;
#1457 = CARTESIAN_POINT ( 'NONE',  ( -0.1749999999999999889, 2.700000000000000178, 1.600000000000000089 ) ) ;
#1458 = VECTOR ( 'NONE', #7416, 1000.000000000000000 ) ;
#1459 = CARTESIAN_POINT ( 'NONE',  ( -2.190084968185500358, -1.567641158900710208, 3.838447030292489792 ) ) ;
#1460 = DIRECTION ( 'NONE',  ( 0.000000000000000000, 0.000000000000000000, -1.000000000000000000 ) ) ;
#1461 = CARTESIAN_POINT ( 'NONE',  ( -1.912899118714301183, -1.381334852594401363, 5.445465495009755408 ) ) ;
#1462 = CARTESIAN_POINT ( 'NONE',  ( 0.1749999999999999889, 8.500000000000000000, -3.200000000000000178 ) ) ;
#1463 = VERTEX_POINT ( 'NONE', #11455 ) ;
#1464 = EDGE_CURVE ( 'NONE', #15033, #3727, #7023, .T. ) ;
#1465 = FACE_OUTER_BOUND ( 'NONE', #13748, .T. ) ;
#1466 = CARTESIAN_POINT ( 'NONE',  ( -2.155845792290839835, -0.5447033898305089217, 3.756158857535780271 ) ) ;
#1467 = VECTOR ( 'NONE', #8980, 1000.000000000000000 ) ;
#1468 = CARTESIAN_POINT ( 'NONE',  ( 0.3413183941262679655, -2.914521003261450360, 7.028571974690709823 ) ) ;
#1469 = LINE ( 'NONE', #2766, #17211 ) ;
#1470 = LINE ( 'NONE', #7205, #4136 ) ;
#1471 = CARTESIAN_POINT ( 'NONE',  ( 2.043014502273419186, -5.041949152542365198, 3.006203457898239062 ) ) ;
#1472 = ORIENTED_EDGE ( 'NONE', *, *, #3297, .F. ) ;
#1473 = ADVANCED_FACE ( 'NONE', ( #1280 ), #12570, .T. ) ;
#1474 = ORIENTED_EDGE ( 'NONE', *, *, #5686, .F. ) ;
#1475 = CARTESIAN_POINT ( 'NONE',  ( -2.340070819011249803, -5.219915254237289304, 4.950151441910548122 ) ) ;
#1476 = EDGE_CURVE ( 'NONE', #16779, #1993, #10429, .T. ) ;
#1477 = CARTESIAN_POINT ( 'NONE',  ( -1.899999999999999911, 4.700000000000000178, 1.600000000000000089 ) ) ;
#1478 = PRODUCT_DEFINITION_FORMATION_WITH_SPECIFIED_SOURCE ( 'ANY', '', #5367, .NOT_KNOWN. ) ;
#1479 = VERTEX_POINT ( 'NONE', #15647 ) ;
#1480 = CARTESIAN_POINT ( 'NONE',  ( -1.752195476665039831, -1.563800282540731779, 6.693219682964347328 ) ) ;
#1481 = SURFACE_STYLE_USAGE ( .BOTH. , #6933 ) ;
#1482 = CARTESIAN_POINT ( 'NONE',  ( 1.873832970144350130, -5.337500000000000355, 2.826167029855650270 ) ) ;
#1483 = VECTOR ( 'NONE', #3233, 1000.000000000000000 ) ;
#1484 = LINE ( 'NONE', #13971, #3607 ) ;
#1485 = CARTESIAN_POINT ( 'NONE',  ( 1.092567884283869972, -0.9621456634052130141, 6.784476218553570526 ) ) ;
#1486 = LINE ( 'NONE', #14059, #12337 ) ;
#1487 = CARTESIAN_POINT ( 'NONE',  ( -1.781655196750479897, -3.520016498756949996, 3.162323035427820450 ) ) ;
#1488 = PLANE ( 'NONE',  #2548 ) ;
#1489 = CARTESIAN_POINT ( 'NONE',  ( -1.777111910197670008, -3.473439922180372452, 3.672004328189223621 ) ) ;
#1490 = PLANE ( 'NONE',  #15912 ) ;
#1491 = ADVANCED_FACE ( 'NONE', ( #5722 ), #12670, .T. ) ;
#1492 = VERTEX_POINT ( 'NONE', #4317 ) ;
#1493 = LINE ( 'NONE', #4342, #15096 ) ;
#1494 = ORIENTED_EDGE ( 'NONE', *, *, #5910, .F. ) ;
#1495 = EDGE_CURVE ( 'NONE', #2828, #5745, #9981, .T. ) ;
#1496 = FACE_OUTER_BOUND ( 'NONE', #9801, .T. ) ;
#1497 = DIRECTION ( 'NONE',  ( 0.000000000000000000, -1.000000000000000000, 0.000000000000000000 ) ) ;
#1498 = ORIENTED_EDGE ( 'NONE', *, *, #12674, .T. ) ;
#1499 = AXIS2_PLACEMENT_3D ( 'NONE', #6840, #4048, #11369 ) ;
#1500 = DIRECTION ( 'NONE',  ( -1.480297366166879989E-16, 0.000000000000000000, 1.000000000000000000 ) ) ;
#1501 = VERTEX_POINT ( 'NONE', #2851 ) ;
#1502 = CARTESIAN_POINT ( 'NONE',  ( 1.580445181003960586, -5.041949152542365198, 3.389704561770334301 ) ) ;
#1503 = CARTESIAN_POINT ( 'NONE',  ( 2.502804106625939440, -2.173136654396201184, 3.817341913956370458 ) ) ;
#1504 = PLANE ( 'NONE',  #16196 ) ;
#1505 = DIRECTION ( 'NONE',  ( 1.000000000000000000, 0.000000000000000000, 0.000000000000000000 ) ) ;
#1506 = DIRECTION ( 'NONE',  ( 0.000000000000000000, -1.000000000000000000, -1.233581138472399909E-16 ) ) ;
#1507 = DIRECTION ( 'NONE',  ( 2.055968564120659776E-16, 1.000000000000000000, 0.000000000000000000 ) ) ;
#1508 = DIRECTION ( 'NONE',  ( 0.7071067811865470176, -0.7071067811865480168, 0.000000000000000000 ) ) ;
#1509 = CARTESIAN_POINT ( 'NONE',  ( -1.850000000000000089, -6.000000000000000000, 2.299999999999999822 ) ) ;
#1510 = VECTOR ( 'NONE', #17453, 1000.000000000000000 ) ;
#1511 = CARTESIAN_POINT ( 'NONE',  ( 2.347833536521260367, -2.541908390648839777, 4.537447324629859224 ) ) ;
#1512 = CARTESIAN_POINT ( 'NONE',  ( -1.333132471082830506, -2.825208726468270370, 6.261300629978947541 ) ) ;
#1513 = CARTESIAN_POINT ( 'NONE',  ( 1.622657008870240762E-16, -3.053113317719175556E-16, 2.649999999999998579 ) ) ;
#1514 = EDGE_CURVE ( 'NONE', #6584, #8504, #14869, .T. ) ;
#1515 = DIRECTION ( 'NONE',  ( -1.189524669241239855E-16, 1.000000000000000000, 0.000000000000000000 ) ) ;
#1516 = PLANE ( 'NONE',  #10324 ) ;
#1517 = VERTEX_POINT ( 'NONE', #160 ) ;
#1518 = EDGE_CURVE ( 'NONE', #15430, #7170, #16730, .T. ) ;
#1519 = CARTESIAN_POINT ( 'NONE',  ( -2.143090896833110381, -0.2046610169491530073, 5.672454929438350391 ) ) ;
#1520 = CARTESIAN_POINT ( 'NONE',  ( -1.710920205120030069, -1.587088570829020107, 6.316012914303580139 ) ) ;
#1521 = ORIENTED_EDGE ( 'NONE', *, *, #4349, .F. ) ;
#1522 = CARTESIAN_POINT ( 'NONE',  ( -4.687608326195109447E-16, -2.220446049250309876E-16, 3.600000000000000089 ) ) ;
#1523 = ORIENTED_EDGE ( 'NONE', *, *, #9000, .F. ) ;
#1524 = CARTESIAN_POINT ( 'NONE',  ( -2.352760675243210198, -3.034803321062869319, 4.757121734156080528 ) ) ;
#1525 = VECTOR ( 'NONE', #14731, 1000.000000000000000 ) ;
#1526 = DIRECTION ( 'NONE',  ( 1.000000000000000000, 0.000000000000000000, 0.000000000000000000 ) ) ;
#1527 = CARTESIAN_POINT ( 'NONE',  ( -2.645377369053839356, -5.528813559322025561, 4.488260618344918740 ) ) ;
#1528 = VERTEX_POINT ( 'NONE', #2672 ) ;
#1529 = ADVANCED_FACE ( 'NONE', ( #4417 ), #4140, .T. ) ;
#1530 = CARTESIAN_POINT ( 'NONE',  ( 1.057242234132090175, -0.3222457627118650025, 2.597442975781520058 ) ) ;
#1531 = ORIENTED_EDGE ( 'NONE', *, *, #1112, .T. ) ;
#1532 = DIRECTION ( 'NONE',  ( -1.908195823574489776E-16, 1.000000000000000000, 1.387778780781449866E-16 ) ) ;
#1533 = DIRECTION ( 'NONE',  ( -6.049014748177265474E-16, -2.081668171172166936E-15, -1.000000000000000000 ) ) ;
#1534 = CARTESIAN_POINT ( 'NONE',  ( 0.6713553523423281266, -2.867944426684881254, 6.640150466718861999 ) ) ;
#1535 = DIRECTION ( 'NONE',  ( -1.480297366166879989E-16, -7.401486830834378990E-17, 1.000000000000000000 ) ) ;
#1536 = ORIENTED_EDGE ( 'NONE', *, *, #2013, .F. ) ;
#1537 = CARTESIAN_POINT ( 'NONE',  ( -0.1881942810071039751, -5.280843314568230085, 2.350674491507239949 ) ) ;
#1538 = DIRECTION ( 'NONE',  ( -0.000000000000000000, 1.000000000000000000, 0.000000000000000000 ) ) ;
#1539 = DIRECTION ( 'NONE',  ( -1.708035422500239940E-16, 1.000000000000000000, 0.000000000000000000 ) ) ;
#1540 = ORIENTED_EDGE ( 'NONE', *, *, #18205, .F. ) ;
#1541 = CARTESIAN_POINT ( 'NONE',  ( 0.005141112625548329915, -0.3685177182334790080, 2.221989741495070003 ) ) ;
#1542 = CARTESIAN_POINT ( 'NONE',  ( -1.980638384804660257, -5.537711864406785978, 4.159858630563765480 ) ) ;
#1543 = CARTESIAN_POINT ( 'NONE',  ( 1.889104232906358982, -0.04449152542372910440, 3.296507079072520607 ) ) ;
#1544 = CARTESIAN_POINT ( 'NONE',  ( 1.477796163681079911, -5.417584745762709986, 6.531563725478140015 ) ) ;
#1545 = PLANE ( 'NONE',  #16760 ) ;
#1546 = EDGE_CURVE ( 'NONE', #12743, #11049, #14241, .T. ) ;
#1547 = ORIENTED_EDGE ( 'NONE', *, *, #6641, .T. ) ;
#1548 = DIRECTION ( 'NONE',  ( 0.000000000000000000, 0.000000000000000000, 1.000000000000000000 ) ) ;
#1549 = CARTESIAN_POINT ( 'NONE',  ( -0.8242394280876599311, -1.171740257999809964, 6.904399023015030501 ) ) ;
#1550 = DIRECTION ( 'NONE',  ( -6.161988852941170860E-64, -1.000000000000000000, 3.773129962568039733E-80 ) ) ;
#1551 = CARTESIAN_POINT ( 'NONE',  ( -1.217499609005920025, -1.707370888630439065, 3.046943272389440960 ) ) ;
#1552 = EDGE_CURVE ( 'NONE', #747, #4341, #7204, .T. ) ;
#1553 = CARTESIAN_POINT ( 'NONE',  ( 2.500000000000000000, 2.799999999999999822, 1.600000000000000089 ) ) ;
#1554 = ORIENTED_EDGE ( 'NONE', *, *, #15046, .T. ) ;
#1555 = EDGE_CURVE ( 'NONE', #6821, #7200, #3033, .T. ) ;
#1556 = CARTESIAN_POINT ( 'NONE',  ( 1.399999999999999911, 5.799999999999999822, 8.300000000000000711 ) ) ;
#1557 = CARTESIAN_POINT ( 'NONE',  ( 2.087380238839969593, -0.4067796610169500116, 6.338810156469096846 ) ) ;
#1558 = CARTESIAN_POINT ( 'NONE',  ( 1.214457691475989920, -3.869340823081270031, 2.684103622926340194 ) ) ;
#1559 = DIRECTION ( 'NONE',  ( 1.000000000000000000, 0.000000000000000000, 0.000000000000000000 ) ) ;
#1560 = DIRECTION ( 'NONE',  ( 1.000000000000000000, 0.000000000000000000, 0.000000000000000000 ) ) ;
#1561 = CARTESIAN_POINT ( 'NONE',  ( -2.268288188848061715, -5.251059322033895249, 3.322421079292323665 ) ) ;
#1562 = EDGE_LOOP ( 'NONE', ( #2488, #15250 ) ) ;
#1563 = ORIENTED_EDGE ( 'NONE', *, *, #7259, .F. ) ;
#1564 = CARTESIAN_POINT ( 'NONE',  ( -1.889999999999999902, 3.500000000000000000, 0.5999999999999999778 ) ) ;
#1565 = CARTESIAN_POINT ( 'NONE',  ( 0.5999999999999999778, 11.40000000000000036, 7.599999999999999645 ) ) ;
#1566 = ORIENTED_EDGE ( 'NONE', *, *, #8695, .F. ) ;
#1567 = CARTESIAN_POINT ( 'NONE',  ( -2.218077401483159683, -4.824160642901089702, 5.486688202856539576 ) ) ;
#1568 = ADVANCED_FACE ( 'NONE', ( #8498 ), #14148, .T. ) ;
#1569 = CARTESIAN_POINT ( 'NONE',  ( 1.349044826018420906, -0.4774152569121725143, 3.148480103883603221 ) ) ;
#1570 = CARTESIAN_POINT ( 'NONE',  ( 0.1749999999999999889, 2.700000000000000178, 1.600000000000000089 ) ) ;
#1571 = LINE ( 'NONE', #3365, #11024 ) ;
#1572 = CARTESIAN_POINT ( 'NONE',  ( -2.337178851518210365, -3.011515032774580103, 4.976298214796809560 ) ) ;
#1573 = EDGE_CURVE ( 'NONE', #5031, #13665, #1469, .T. ) ;
#1574 = DIRECTION ( 'NONE',  ( -4.898587196589410857E-16, -1.000000000000000000, 2.696301922142130194E-31 ) ) ;
#1575 = CARTESIAN_POINT ( 'NONE',  ( 0.1768565782245979934, -3.752899381639830168, 2.353200596935780098 ) ) ;
#1576 = EDGE_CURVE ( 'NONE', #10192, #8619, #11922, .T. ) ;
#1577 = FACE_OUTER_BOUND ( 'NONE', #10755, .T. ) ;
#1578 = EDGE_CURVE ( 'NONE', #6801, #1039, #77, .T. ) ;
#1579 = CARTESIAN_POINT ( 'NONE',  ( 2.018065005288410152, -4.172088570829024512, 5.077247235985069551 ) ) ;
#1580 = LINE ( 'NONE', #12786, #17918 ) ;
#1581 = ADVANCED_FACE ( 'NONE', ( #7289 ), #12935, .T. ) ;
#1582 = ORIENTED_EDGE ( 'NONE', *, *, #9764, .F. ) ;
#1583 = DIRECTION ( 'NONE',  ( 0.000000000000000000, 0.000000000000000000, 1.000000000000000000 ) ) ;
#1584 = ORIENTED_EDGE ( 'NONE', *, *, #13908, .T. ) ;
#1585 = DIRECTION ( 'NONE',  ( -5.921189464667500234E-16, 9.860761315262649757E-32, -1.000000000000000000 ) ) ;
#1586 = VECTOR ( 'NONE', #9798, 1000.000000000000000 ) ;
#1587 = CARTESIAN_POINT ( 'NONE',  ( 0.5500000000000000444, 3.050000000000000266, 2.699264068711930253 ) ) ;
#1588 = VERTEX_POINT ( 'NONE', #13026 ) ;
#1589 = CARTESIAN_POINT ( 'NONE',  ( 6.735557395310439065E-16, -5.500000000000000000, -3.367778697655220026E-16 ) ) ;
#1590 = VERTEX_POINT ( 'NONE', #6167 ) ;
#1591 = EDGE_CURVE ( 'NONE', #4752, #1389, #4856, .T. ) ;
#1592 = CARTESIAN_POINT ( 'NONE',  ( -1.489797906646480596, -5.488771186440680516, 6.112509577910826941 ) ) ;
#1593 = EDGE_CURVE ( 'NONE', #11546, #16860, #17258, .T. ) ;
#1594 = DIRECTION ( 'NONE',  ( -8.269460797427580527E-16, 0.000000000000000000, 1.000000000000000000 ) ) ;
#1595 = DIRECTION ( 'NONE',  ( 1.000000000000000000, 0.000000000000000000, 0.000000000000000000 ) ) ;
#1596 = DIRECTION ( 'NONE',  ( -1.224646799147350002E-16, 1.000000000000000000, 6.123233995736759873E-17 ) ) ;
#1597 = FACE_OUTER_BOUND ( 'NONE', #2516, .T. ) ;
#1598 = EDGE_CURVE ( 'NONE', #17652, #5170, #13115, .T. ) ;
#1599 = CARTESIAN_POINT ( 'NONE',  ( -1.800000000000000044, 0.5999999999999999778, 6.599999999999999645 ) ) ;
#1600 = DIRECTION ( 'NONE',  ( 1.593283298565159857E-16, -1.000000000000000000, -3.186566597130310346E-16 ) ) ;
#1601 = CARTESIAN_POINT ( 'NONE',  ( -1.044181395669830259, -2.052854336594790219, 2.590869634085910089 ) ) ;
#1602 = CARTESIAN_POINT ( 'NONE',  ( -0.7616804549307533145, -3.337551068810613142, 2.793499350326739350 ) ) ;
#1603 = CARTESIAN_POINT ( 'NONE',  ( -1.661700935788390066, -0.2625000000000000111, 3.038299064211610112 ) ) ;
#1604 = DIRECTION ( 'NONE',  ( 1.000000000000000000, 0.000000000000000000, -3.097720492815726673E-16 ) ) ;
#1605 = CARTESIAN_POINT ( 'NONE',  ( -1.000000000000000000, -5.500000000000000000, 5.100000000000000533 ) ) ;
#1606 = ORIENTED_EDGE ( 'NONE', *, *, #16883, .T. ) ;
#1607 = CARTESIAN_POINT ( 'NONE',  ( 1.764807890102179977, -2.378890372630820149, 3.143016121304719857 ) ) ;
#1608 = AXIS2_PLACEMENT_3D ( 'NONE', #4439, #8701, #12962 ) ;
#1609 = ORIENTED_EDGE ( 'NONE', *, *, #6412, .T. ) ;
#1610 = ORIENTED_EDGE ( 'NONE', *, *, #10246, .F. ) ;
#1611 = ADVANCED_FACE ( 'NONE', ( #7472 ), #10151, .T. ) ;
#1612 = CARTESIAN_POINT ( 'NONE',  ( 1.003115764947319244, -4.106064582324130185, 6.828967930617569237 ) ) ;
#1613 = PRODUCT_CONTEXT ( 'NONE', #4584, 'mechanical' ) ;
#1614 = CARTESIAN_POINT ( 'NONE',  ( -1.428515267734880023, -5.568855932203390147, 2.829745655876930055 ) ) ;
#1615 = ORIENTED_EDGE ( 'NONE', *, *, #4010, .T. ) ;
#1616 = CARTESIAN_POINT ( 'NONE',  ( 1.042222075699120287, -0.4245762711864407013, 6.468743694056166227 ) ) ;
#1617 = ORIENTED_EDGE ( 'NONE', *, *, #12083, .T. ) ;
#1618 = EDGE_CURVE ( 'NONE', #1835, #3272, #11543, .T. ) ;
#1619 = CARTESIAN_POINT ( 'NONE',  ( -0.5500000000000000444, 6.450000000000000178, 3.600000000000000089 ) ) ;
#1620 = DIRECTION ( 'NONE',  ( 0.000000000000000000, 1.000000000000000000, 1.332267629550190018E-15 ) ) ;
#1621 = AXIS2_PLACEMENT_3D ( 'NONE', #12401, #10925, #15275 ) ;
#1622 = CARTESIAN_POINT ( 'NONE',  ( -0.9976707306414490661, -3.077539021279473097, 6.494311833503151554 ) ) ;
#1623 = ORIENTED_EDGE ( 'NONE', *, *, #5769, .T. ) ;
#1624 = CARTESIAN_POINT ( 'NONE',  ( -1.500000000000000000, -6.000000000000000000, 2.299999999999999822 ) ) ;
#1625 = CARTESIAN_POINT ( 'NONE',  ( 1.983927814618709873E-15, 10.80000000000000071, 7.700000000000000178 ) ) ;
#1626 = ORIENTED_EDGE ( 'NONE', *, *, #7917, .T. ) ;
#1627 = LINE ( 'NONE', #4660, #6210 ) ;
#1628 = CARTESIAN_POINT ( 'NONE',  ( -1.901882987994748975, -5.506567796610171150, 5.472995608211450147 ) ) ;
#1629 = FACE_OUTER_BOUND ( 'NONE', #6040, .T. ) ;
#1630 = CARTESIAN_POINT ( 'NONE',  ( -1.300961508564169700, -0.1779661016949160290, 6.661123742937278713 ) ) ;
#1631 = CARTESIAN_POINT ( 'NONE',  ( -0.9000000000000000222, 2.050000000000000266, 3.600000000000000089 ) ) ;
#1632 = ORIENTED_EDGE ( 'NONE', *, *, #6290, .T. ) ;
#1633 = DIRECTION ( 'NONE',  ( 0.000000000000000000, 0.000000000000000000, 1.000000000000000000 ) ) ;
#1634 = CARTESIAN_POINT ( 'NONE',  ( -1.026235786675429917, -1.195028546288090077, 6.817920158464570335 ) ) ;
#1635 = VECTOR ( 'NONE', #13186, 1000.000000000000000 ) ;
#1636 = CARTESIAN_POINT ( 'NONE',  ( -1.899999999999999911, 2.799999999999999822, 1.600000000000000089 ) ) ;
#1637 = CARTESIAN_POINT ( 'NONE',  ( 1.555285212483259683, -2.079983501243050981, 3.359854578615069087 ) ) ;
#1638 = DIRECTION ( 'NONE',  ( -4.476422471267237545E-17, -0.6823182503600040416, -0.7310552682428754778 ) ) ;
#1639 = VERTEX_POINT ( 'NONE', #10502 ) ;
#1640 = CARTESIAN_POINT ( 'NONE',  ( -2.191755591049691532, -0.5536016949152540167, 3.203650300307721466 ) ) ;
#1641 = CARTESIAN_POINT ( 'NONE',  ( 2.100188519621589922, -4.009070552810999999, 3.637948273607370275 ) ) ;
#1642 = DIRECTION ( 'NONE',  ( 1.000000000000000000, 0.000000000000000000, 0.000000000000000000 ) ) ;
#1643 = DIRECTION ( 'NONE',  ( -3.700743415417199972E-16, 1.000000000000000000, 3.581736239852560511E-31 ) ) ;
#1644 = CARTESIAN_POINT ( 'NONE',  ( -0.9664230948142090716, -5.282203389830510076, 2.228384861502259895 ) ) ;
#1645 = EDGE_LOOP ( 'NONE', ( #6162, #8005, #2854, #8704 ) ) ;
#1646 = ORIENTED_EDGE ( 'NONE', *, *, #7536, .F. ) ;
#1647 = CARTESIAN_POINT ( 'NONE',  ( -1.248294325655369796, -5.273305084745759430, 2.704938983774311190 ) ) ;
#1648 =( LENGTH_UNIT ( ) NAMED_UNIT ( * ) SI_UNIT ( .MILLI., .METRE. ) );
#1649 = CARTESIAN_POINT ( 'NONE',  ( 1.652654650382400003, -0.7952867690272209522, 3.029252778805629820 ) ) ;
#1650 = VERTEX_POINT ( 'NONE', #264 ) ;
#1651 = CARTESIAN_POINT ( 'NONE',  ( 2.418933091173299577, -1.098034516774970770, 5.791730916219126613 ) ) ;
#1652 = CARTESIAN_POINT ( 'NONE',  ( 0.1953673232040119001, -0.6247245358507567126, 2.648920247487680513 ) ) ;
#1653 = DIRECTION ( 'NONE',  ( -1.000000000000000000, -1.233581138472399909E-16, -1.480297366166879989E-16 ) ) ;
#1654 = CARTESIAN_POINT ( 'NONE',  ( -0.7678268402137429227, -2.732055573315119723, 6.924676972266150088 ) ) ;
#1655 = CARTESIAN_POINT ( 'NONE',  ( 1.873832970144350130, -5.037500000000000533, 2.826167029855650270 ) ) ;
#1656 = CARTESIAN_POINT ( 'NONE',  ( -2.380466601827099016, -1.889836318576769036, 3.526759849567179916 ) ) ;
#1657 = CARTESIAN_POINT ( 'NONE',  ( -0.5500000000000000444, 6.450000000000000178, 1.600000000000000089 ) ) ;
#1658 = CARTESIAN_POINT ( 'NONE',  ( -4.898587196589400133E-17, 5.318248954186070243, 6.599999999999999645 ) ) ;
#1659 = CARTESIAN_POINT ( 'NONE',  ( -0.9516466452860307124, -4.637854336594775084, 6.519140045500596337 ) ) ;
#1660 = VECTOR ( 'NONE', #6566, 1000.000000000000000 ) ;
#1661 = CARTESIAN_POINT ( 'NONE',  ( 1.850000000000000089, 11.25000000000000000, 7.700000000000000178 ) ) ;
#1662 = CARTESIAN_POINT ( 'NONE',  ( -1.899999999999999911, 7.299999999999999822, 1.600000000000000089 ) ) ;
#1663 = VERTEX_POINT ( 'NONE', #10418 ) ;
#1664 = TOROIDAL_SURFACE ( 'NONE', #9645, 0.2999999999999999889, 0.2500000000000000000 ) ;
#1665 = EDGE_CURVE ( 'NONE', #10455, #4443, #7648, .T. ) ;
#1666 = CARTESIAN_POINT ( 'NONE',  ( 3.673940397442059498E-17, 2.600000000000000089, 8.000000000000000000 ) ) ;
#1667 = ORIENTED_EDGE ( 'NONE', *, *, #711, .F. ) ;
#1668 = DIRECTION ( 'NONE',  ( -2.242874797222529735E-16, 0.000000000000000000, -1.000000000000000000 ) ) ;
#1669 = ADVANCED_FACE ( 'NONE', ( #11908 ), #17176, .T. ) ;
#1670 = ORIENTED_EDGE ( 'NONE', *, *, #5013, .F. ) ;
#1671 = EDGE_CURVE ( 'NONE', #17897, #14849, #14414, .T. ) ;
#1672 = CARTESIAN_POINT ( 'NONE',  ( 2.051331987628511211, -5.373093220338980736, 4.618035453557344461 ) ) ;
#1673 = EDGE_CURVE ( 'NONE', #14845, #9755, #3464, .T. ) ;
#1674 = CARTESIAN_POINT ( 'NONE',  ( -1.899999999999999911, 2.000000000000000000, 0.5999999999999999778 ) ) ;
#1675 = CARTESIAN_POINT ( 'NONE',  ( -1.720450724489941852, -2.825208726468270370, 6.720683794561613134 ) ) ;
#1676 = DIRECTION ( 'NONE',  ( -1.224646799147350002E-16, 1.000000000000000000, 6.123233995736769734E-17 ) ) ;
#1677 = CARTESIAN_POINT ( 'NONE',  ( -0.009452110982656913851, -5.299807955295455564, 2.050000000000001155 ) ) ;
#1678 = CLOSED_SHELL ( 'NONE', ( #17250, #10957, #2235, #14129, #6811, #13216, #6897, #6200, #5319, #10041, #4520, #3704, #315, #105, #14666, #4593, #6660, #13195, #5516, #8926, #8648, #17271, #17198, #13006, #14621, #3585, #15481, #18027, #12510, #4723, #2807, #4042, #259, #18212, #2599, #5995, #17741, #11109, #16494, #11392, #3802, #17042, #12519, #13359, #813, #8455, #15528, #1529, #7562, #16316, #5674, #14159, #4712, #1990, #14350, #3991, #1110, #8864, #17976, #15869, #16128, #17491, #15822, #8789, #13718, #3819, #16655, #8044, #598, #16948, #7270, #8598 ) ) ;
#1679 = VECTOR ( 'NONE', #7092, 1000.000000000000000 ) ;
#1680 = CARTESIAN_POINT ( 'NONE',  ( 2.616666666666669805, 1.110223024625159992E-16, 7.649999999999999467 ) ) ;
#1681 = CARTESIAN_POINT ( 'NONE',  ( 4.898587196589403214E-17, 2.600000000000000089, 7.700000000000000178 ) ) ;
#1682 = CARTESIAN_POINT ( 'NONE',  ( -2.237394498046660019, -3.263845327585780165, 5.429939413646380331 ) ) ;
#1683 = CARTESIAN_POINT ( 'NONE',  ( -0.8014931112106958855, -4.315659176918716255, 6.590108630558016323 ) ) ;
#1684 = CARTESIAN_POINT ( 'NONE',  ( -2.351526912647309953, -0.2269067796610169940, 4.606040641882809261 ) ) ;
#1685 = CARTESIAN_POINT ( 'NONE',  ( 1.899999999999999911, 2.799999999999999822, 1.600000000000000089 ) ) ;
#1686 = AXIS2_PLACEMENT_3D ( 'NONE', #2093, #6340, #17621 ) ;
#1687 = DIRECTION ( 'NONE',  ( -1.000000000000000000, 0.000000000000000000, 2.220446049250309876E-16 ) ) ;
#1688 = CARTESIAN_POINT ( 'NONE',  ( 2.329383452786330189, -1.028169651910100013, 5.035735636132829818 ) ) ;
#1689 = ORIENTED_EDGE ( 'NONE', *, *, #1555, .F. ) ;
#1690 = CARTESIAN_POINT ( 'NONE',  ( 2.556942001999820580, -3.756740257999804378, 3.989253004641562406 ) ) ;
#1691 = CARTESIAN_POINT ( 'NONE',  ( 1.846259792136599076, -0.05338983050847485173, 3.802221692020924415 ) ) ;
#1692 = CARTESIAN_POINT ( 'NONE',  ( -1.741913176380149864, -1.959701183441629802, 3.117443785062560035 ) ) ;
#1693 = ORIENTED_EDGE ( 'NONE', *, *, #17999, .T. ) ;
#1694 = EDGE_CURVE ( 'NONE', #7811, #5515, #8860, .T. ) ;
#1695 = VECTOR ( 'NONE', #2486, 1000.000000000000114 ) ;
#1696 = VERTEX_POINT ( 'NONE', #11628 ) ;
#1697 = CARTESIAN_POINT ( 'NONE',  ( -0.7109160811435618621, -4.292370888630430592, 6.943511536198419876 ) ) ;
#1698 = APPLICATION_PROTOCOL_DEFINITION ( 'draft international standard', 'automotive_design', 1998, #13728 ) ;
#1699 = CARTESIAN_POINT ( 'NONE',  ( -2.087380238839969593, -5.193220338983044471, 6.338810156469112833 ) ) ;
#1700 = EDGE_LOOP ( 'NONE', ( #16082, #7539, #16921, #5146, #2357, #9848 ) ) ;
#1701 = CARTESIAN_POINT ( 'NONE',  ( -1.899999999999999911, -3.954861110236189622E-16, 3.278889744907200310 ) ) ;
#1702 = AXIS2_PLACEMENT_3D ( 'NONE', #8992, #14640, #1954 ) ;
#1703 = CARTESIAN_POINT ( 'NONE',  ( 2.041338374031088865, -0.3800847457627119508, 4.918217215283659627 ) ) ;
#1704 = AXIS2_PLACEMENT_3D ( 'NONE', #13351, #1798, #7705 ) ;
#1705 = ORIENTED_EDGE ( 'NONE', *, *, #7576, .T. ) ;
#1706 = PLANE ( 'NONE',  #482 ) ;
#1707 = DIRECTION ( 'NONE',  ( -2.018587317500279868E-16, 1.000000000000000000, 0.000000000000000000 ) ) ;
#1708 = CARTESIAN_POINT ( 'NONE',  ( 1.538437905834991515, -2.378890372630820149, 3.340547664492009350 ) ) ;
#1709 = AXIS2_PLACEMENT_3D ( 'NONE', #7640, #1978, #11621 ) ;
#1710 = VERTEX_POINT ( 'NONE', #7389 ) ;
#1711 = CARTESIAN_POINT ( 'NONE',  ( 1.399999999999999911, -5.000000000000000000, 6.100000000000000533 ) ) ;
#1712 = VECTOR ( 'NONE', #18175, 1000.000000000000000 ) ;
#1713 = CARTESIAN_POINT ( 'NONE',  ( 2.500000000000000000, 4.700000000000000178, 0.6099999999999999867 ) ) ;
#1714 = VECTOR ( 'NONE', #925, 1000.000000000000000 ) ;
#1715 = CARTESIAN_POINT ( 'NONE',  ( 1.647523294046493447, -5.038055510066682174, 3.052476705953498737 ) ) ;
#1716 = ORIENTED_EDGE ( 'NONE', *, *, #8682, .F. ) ;
#1717 = AXIS2_PLACEMENT_3D ( 'NONE', #12010, #13305, #14785 ) ;
#1718 = CARTESIAN_POINT ( 'NONE',  ( 2.500000000000000000, 4.700000000000000178, 1.600000000000000089 ) ) ;
#1719 = VECTOR ( 'NONE', #13446, 1000.000000000000000 ) ;
#1720 = EDGE_CURVE ( 'NONE', #13413, #7434, #16161, .T. ) ;
#1721 = CARTESIAN_POINT ( 'NONE',  ( 0.3743405594629509725, -0.1423728813559329565, 7.023440622744399953 ) ) ;
#1722 = CARTESIAN_POINT ( 'NONE',  ( -1.685497504775380850, -0.2673043920988010802, 2.637581209070348987 ) ) ;
#1723 = CARTESIAN_POINT ( 'NONE',  ( 2.471388659209138972, -4.218665147405589622, 5.667135868497455320 ) ) ;
#1724 = ORIENTED_EDGE ( 'NONE', *, *, #5093, .T. ) ;
#1725 = VECTOR ( 'NONE', #10887, 1000.000000000000000 ) ;
#1726 = DIRECTION ( 'NONE',  ( 2.220446049250309876E-16, 0.000000000000000000, -1.000000000000000000 ) ) ;
#1727 = VECTOR ( 'NONE', #3209, 1000.000000000000000 ) ;
#1728 = CARTESIAN_POINT ( 'NONE',  ( 0.6918414964981909332, -1.940253771513320125, 2.450533167346750307 ) ) ;
#1729 = EDGE_CURVE ( 'NONE', #12906, #17929, #11720, .T. ) ;
#1730 = FACE_OUTER_BOUND ( 'NONE', #9445, .T. ) ;
#1731 = CARTESIAN_POINT ( 'NONE',  ( -1.810994336139479133, -2.918361879621429011, 5.667058093962724641 ) ) ;
#1732 = AXIS2_PLACEMENT_3D ( 'NONE', #4990, #13511, #6471 ) ;
#1733 = CARTESIAN_POINT ( 'NONE',  ( -0.1749999999999999889, 7.500000000000000000, 1.600000000000000089 ) ) ;
#1734 = DIRECTION ( 'NONE',  ( 1.073215590470990073E-14, 1.000000000000000000, 0.000000000000000000 ) ) ;
#1735 = VERTEX_POINT ( 'NONE', #14508 ) ;
#1736 = AXIS2_PLACEMENT_3D ( 'NONE', #2727, #12529, #18142 ) ;
#1737 = CARTESIAN_POINT ( 'NONE',  ( 1.850000000000000089, -5.599999999999999645, 2.299999999999999822 ) ) ;
#1738 = CARTESIAN_POINT ( 'NONE',  ( -2.325590009395030133, -4.870737219477670799, 5.061077271074069905 ) ) ;
#1739 = DIRECTION ( 'NONE',  ( 1.110223024625159992E-16, 0.000000000000000000, -1.000000000000000000 ) ) ;
#1740 = PLANE ( 'NONE',  #16577 ) ;
#1741 = CARTESIAN_POINT ( 'NONE',  ( -2.601107615185130673, -5.215466101694915757, 5.226397344856384741 ) ) ;
#1742 = ORIENTED_EDGE ( 'NONE', *, *, #3121, .F. ) ;
#1743 = ADVANCED_FACE ( 'NONE', ( #3302 ), #17353, .T. ) ;
#1744 = VERTEX_POINT ( 'NONE', #1906 ) ;
#1745 = CARTESIAN_POINT ( 'NONE',  ( -1.899999999999999911, -2.607830583485239887E-17, -2.799999999999999822 ) ) ;
#1746 =( LENGTH_UNIT ( ) NAMED_UNIT ( * ) SI_UNIT ( .MILLI., .METRE. ) );
#1747 = AXIS2_PLACEMENT_3D ( 'NONE', #7958, #13604, #17827 ) ;
#1748 = DIRECTION ( 'NONE',  ( 3.330669073875480271E-15, 1.000000000000000000, 3.700743415417199972E-16 ) ) ;
#1749 = CIRCLE ( 'NONE', #15946, 0.1000000000000000472 ) ;
#1750 = ORIENTED_EDGE ( 'NONE', *, *, #5753, .T. ) ;
#1751 = AXIS2_PLACEMENT_3D ( 'NONE', #9938, #10196, #1526 ) ;
#1752 = CARTESIAN_POINT ( 'NONE',  ( 1.741105240696918965, -0.4774152569121725143, 2.691996915772988608 ) ) ;
#1753 = DIRECTION ( 'NONE',  ( 1.306144734853129823E-16, -1.000000000000000000, -1.306144734853129823E-16 ) ) ;
#1754 = CARTESIAN_POINT ( 'NONE',  ( 2.283153923255319739, -2.196424942684489512, 4.129076318403449797 ) ) ;
#1755 = CARTESIAN_POINT ( 'NONE',  ( 0.2735655355027601376, -5.004947479095214646, 2.050775599341920330 ) ) ;
#1756 = CARTESIAN_POINT ( 'NONE',  ( -2.352190863465239978, -4.917313796054239461, 4.622903765856379188 ) ) ;
#1757 = AXIS2_PLACEMENT_3D ( 'NONE', #13488, #6446, #5062 ) ;
#1758 = DIRECTION ( 'NONE',  ( -1.000000000000000000, 0.000000000000000000, 0.000000000000000000 ) ) ;
#1759 = CARTESIAN_POINT ( 'NONE',  ( 1.936998685628529948, -0.8418633456037969420, 3.363294429306519895 ) ) ;
#1760 = LINE ( 'NONE', #14260, #16505 ) ;
#1761 = DIRECTION ( 'NONE',  ( 1.000000000000000000, 0.000000000000000000, 4.440892098500630106E-16 ) ) ;
#1762 = ORIENTED_EDGE ( 'NONE', *, *, #7277, .F. ) ;
#1763 = ORIENTED_EDGE ( 'NONE', *, *, #9516, .T. ) ;
#1764 = LINE ( 'NONE', #7410, #15311 ) ;
#1765 = CARTESIAN_POINT ( 'NONE',  ( 1.899999999999999911, 9.199999999999999289, 0.5999999999999999778 ) ) ;
#1766 = ORIENTED_EDGE ( 'NONE', *, *, #11413, .T. ) ;
#1767 = AXIS2_PLACEMENT_3D ( 'NONE', #14108, #8469, #1436 ) ;
#1768 = CARTESIAN_POINT ( 'NONE',  ( -1.821706171509118954, -5.502118644067805597, 5.646608543709410455 ) ) ;
#1769 = LINE ( 'NONE', #15841, #1458 ) ;
#1770 = CARTESIAN_POINT ( 'NONE',  ( -2.308170020371289599, -1.726818300558750074, 5.159452766389659217 ) ) ;
#1771 = CARTESIAN_POINT ( 'NONE',  ( 2.523518139275831462, -2.336154672414218592, 5.521565513971776085 ) ) ;
#1772 = DIRECTION ( 'NONE',  ( -6.083413833562510128E-16, 1.520853458390629997E-16, -1.000000000000000000 ) ) ;
#1773 = DIRECTION ( 'NONE',  ( -1.000000000000000000, 0.000000000000000000, 0.000000000000000000 ) ) ;
#1774 = PLANE ( 'NONE',  #4022 ) ;
#1775 = CARTESIAN_POINT ( 'NONE',  ( 1.899999999999999911, 0.5999999999999999778, 7.599999999999999645 ) ) ;
#1776 = CARTESIAN_POINT ( 'NONE',  ( 1.800000000000000044, 11.40000000000000036, 7.550000000000000711 ) ) ;
#1777 = CARTESIAN_POINT ( 'NONE',  ( -2.062913653388399826, -3.217268751009200400, 5.832754583370829415 ) ) ;
#1778 = CARTESIAN_POINT ( 'NONE',  ( -1.292934267244330471, -4.385524041783587457, 6.294748514096648151 ) ) ;
#1779 =( REPRESENTATION_RELATIONSHIP ('NONE','NONE', #2757, #4614 ) REPRESENTATION_RELATIONSHIP_WITH_TRANSFORMATION ( #1870 )SHAPE_REPRESENTATION_RELATIONSHIP( ) );
#1780 = EDGE_CURVE ( 'NONE', #11214, #475, #7552, .T. ) ;
#1781 = CARTESIAN_POINT ( 'NONE',  ( 0.009452039534068971960, -5.000193177104105047, 2.350000000173209536 ) ) ;
#1782 = EDGE_CURVE ( 'NONE', #14972, #12624, #14670, .T. ) ;
#1783 = VECTOR ( 'NONE', #451, 1000.000000000000114 ) ;
#1784 = CARTESIAN_POINT ( 'NONE',  ( 2.226511124464869873, -1.074746228486680000, 5.462491901673799610 ) ) ;
#1785 = VERTEX_POINT ( 'NONE', #612 ) ;
#1786 = CARTESIAN_POINT ( 'NONE',  ( 1.176011442874370649, -3.547145663405211646, 2.320901267448020722 ) ) ;
#1787 = CARTESIAN_POINT ( 'NONE',  ( 1.725722849164588624, -0.1023305084745770588, 5.812007984777676661 ) ) ;
#1788 = CARTESIAN_POINT ( 'NONE',  ( -2.267872052190610166, -1.843259742000189938, 4.071110468860649867 ) ) ;
#1789 = EDGE_LOOP ( 'NONE', ( #12555, #11012, #7801, #5145 ) ) ;
#1790 = ORIENTED_EDGE ( 'NONE', *, *, #16946, .T. ) ;
#1791 = CARTESIAN_POINT ( 'NONE',  ( 2.500000000000000000, 0.8000000000000000444, -1.769429514865259726E-15 ) ) ;
#1792 = VERTEX_POINT ( 'NONE', #13383 ) ;
#1793 = CARTESIAN_POINT ( 'NONE',  ( 0.3752419433107367919, -4.175929447188990729, 7.023346545710360544 ) ) ;
#1794 = PRODUCT_CONTEXT ( 'NONE', #2381, 'mechanical' ) ;
#1795 = CARTESIAN_POINT ( 'NONE',  ( 1.254903241568450900, -5.126483050847465250, 7.038391080368498365 ) ) ;
#1796 = ORIENTED_EDGE ( 'NONE', *, *, #9182, .T. ) ;
#1797 = EDGE_CURVE ( 'NONE', #17265, #4743, #6333, .T. ) ;
#1798 = DIRECTION ( 'NONE',  ( 1.224646799147350002E-16, -1.000000000000000000, -6.123233995736769734E-17 ) ) ;
#1799 = VECTOR ( 'NONE', #6073, 1000.000000000000000 ) ;
#1800 = CARTESIAN_POINT ( 'NONE',  ( -1.112838723655040107, -0.4735169491525429986, 6.773667561836210105 ) ) ;
#1801 = VERTEX_POINT ( 'NONE', #697 ) ;
#1802 = EDGE_CURVE ( 'NONE', #16922, #8308, #12441, .T. ) ;
#1803 = CARTESIAN_POINT ( 'NONE',  ( -0.1749999999999999889, 7.799999999999999822, 0.4000000000000000222 ) ) ;
#1804 = CARTESIAN_POINT ( 'NONE',  ( -1.399999999999999911, -5.500000000000000000, 6.100000000000000533 ) ) ;
#1805 = CARTESIAN_POINT ( 'NONE',  ( -1.160665242129840014, -3.100827309567759205, 6.393445611273007145 ) ) ;
#1806 = EDGE_CURVE ( 'NONE', #17781, #14972, #8098, .T. ) ;
#1807 = CARTESIAN_POINT ( 'NONE',  ( 1.407651048079441525, -0.02669491525423760975, 2.450250343405061759 ) ) ;
#1808 = ORIENTED_EDGE ( 'NONE', *, *, #10536, .F. ) ;
#1809 = EDGE_CURVE ( 'NONE', #9985, #14961, #5402, .T. ) ;
#1810 = DIRECTION ( 'NONE',  ( 1.306144734853129823E-16, -1.000000000000000000, -1.306144734853129823E-16 ) ) ;
#1811 = EDGE_CURVE ( 'NONE', #12303, #13228, #11997, .T. ) ;
#1812 = ORIENTED_EDGE ( 'NONE', *, *, #1495, .F. ) ;
#1813 = VECTOR ( 'NONE', #4502, 1000.000000000000000 ) ;
#1814 = CARTESIAN_POINT ( 'NONE',  ( -0.5921572875253819923, 6.450000000000000178, 1.600000000000000089 ) ) ;
#1815 = CARTESIAN_POINT ( 'NONE',  ( -0.9222751404131109831, -5.577754237288145234, 2.865854510788139908 ) ) ;
#1816 = DIRECTION ( 'NONE',  ( -2.220446049250309876E-16, 0.000000000000000000, 1.000000000000000000 ) ) ;
#1817 = CARTESIAN_POINT ( 'NONE',  ( 2.608006145151101407, -4.172088570829024512, 5.191342690854350295 ) ) ;
#1818 = ORIENTED_EDGE ( 'NONE', *, *, #1042, .T. ) ;
#1819 = CARTESIAN_POINT ( 'NONE',  ( 2.005512128484129963, -3.686875393134939394, 3.468469736471340159 ) ) ;
#1820 = DIRECTION ( 'NONE',  ( 2.936127007273139866E-16, 0.000000000000000000, -1.000000000000000000 ) ) ;
#1821 = CARTESIAN_POINT ( 'NONE',  ( -2.007801995112629356, -2.988226744486289999, 5.128524201241715375 ) ) ;
#1822 = EDGE_CURVE ( 'NONE', #12759, #5909, #10605, .T. ) ;
#1823 = CARTESIAN_POINT ( 'NONE',  ( -0.5999999999999999778, 0.5999999999999999778, 7.599999999999999645 ) ) ;
#1824 = ORIENTED_EDGE ( 'NONE', *, *, #10961, .T. ) ;
#1825 = FACE_OUTER_BOUND ( 'NONE', #59, .T. ) ;
#1826 = DIRECTION ( 'NONE',  ( -2.775557561562890365E-16, -1.000000000000000000, -2.775557561562890365E-16 ) ) ;
#1827 = CARTESIAN_POINT ( 'NONE',  ( -2.370419177058770366, -1.358046564306109261, 5.893409660608596390 ) ) ;
#1828 = CARTESIAN_POINT ( 'NONE',  ( -1.496290472746829803, -0.5672554343907050267, 2.872674968141029961 ) ) ;
#1829 = DIRECTION ( 'NONE',  ( 6.123233995736764803E-17, 1.000000000000000000, 0.000000000000000000 ) ) ;
#1830 = DIRECTION ( 'NONE',  ( 0.3420201433256691015, 0.000000000000000000, -0.9396926207859082059 ) ) ;
#1831 = CARTESIAN_POINT ( 'NONE',  ( 1.943632316591230147, -5.046398305084740521, 3.373048379518159834 ) ) ;
#1832 = VERTEX_POINT ( 'NONE', #897 ) ;
#1833 = ORIENTED_EDGE ( 'NONE', *, *, #8135, .F. ) ;
#1834 = DIRECTION ( 'NONE',  ( 1.000000000000000000, 0.000000000000000000, 0.000000000000000000 ) ) ;
#1835 = VERTEX_POINT ( 'NONE', #6793 ) ;
#1836 = EDGE_CURVE ( 'NONE', #12743, #12376, #17613, .T. ) ;
#1837 = CARTESIAN_POINT ( 'NONE',  ( 2.635341251434490495, -2.588484967225421762, 5.013193520829454464 ) ) ;
#1838 = CARTESIAN_POINT ( 'NONE',  ( 1.495970331552388455, -0.4480353997208171291, 2.495424373718078570 ) ) ;
#1839 = DIRECTION ( 'NONE',  ( -1.000000000000000000, 0.000000000000000000, 0.000000000000000000 ) ) ;
#1840 = EDGE_CURVE ( 'NONE', #10043, #4420, #5695, .T. ) ;
#1841 = CARTESIAN_POINT ( 'NONE',  ( 2.295719155670170153, -2.312866384125930264, 5.218091927917190453 ) ) ;
#1843 = EDGE_CURVE ( 'NONE', #12160, #16040, #15323, .T. ) ;
#1842 = DIRECTION ( 'NONE',  ( -0.7071067811865470176, 0.000000000000000000, -0.7071067811865480168 ) ) ;
#1844 = CARTESIAN_POINT ( 'NONE',  ( 2.185196738168471153, -0.8418633456037974971, 3.194002352996649474 ) ) ;
#1845 = CARTESIAN_POINT ( 'NONE',  ( 2.500000000000000000, 10.00000000000000000, 0.5999999999999999778 ) ) ;
#1846 = CARTESIAN_POINT ( 'NONE',  ( -2.049150047780149642, -4.894025507765944916, 4.826039376028564476 ) ) ;
#1847 = CARTESIAN_POINT ( 'NONE',  ( -1.899999999999999911, 10.00000000000000000, 0.5999999999999999778 ) ) ;
#1848 = PLANE ( 'NONE',  #7110 ) ;
#1849 = ORIENTED_EDGE ( 'NONE', *, *, #2013, .T. ) ;
#1850 = CARTESIAN_POINT ( 'NONE',  ( -1.250000000000000000, 0.5999999999999999778, 7.599999999999999645 ) ) ;
#1851 = ORIENTED_EDGE ( 'NONE', *, *, #17367, .T. ) ;
#1852 = CARTESIAN_POINT ( 'NONE',  ( -0.5500000000000000444, 2.050000000000000266, 1.600000000000000089 ) ) ;
#1853 = CARTESIAN_POINT ( 'NONE',  ( -1.889999999999999902, 8.500000000000000000, 0.5999999999999999778 ) ) ;
#1854 = ORIENTED_EDGE ( 'NONE', *, *, #13294, .F. ) ;
#1855 = CARTESIAN_POINT ( 'NONE',  ( -1.417709711196470046, -2.006277760018209566, 2.821478011237799954 ) ) ;
#1856 = CARTESIAN_POINT ( 'NONE',  ( -3.061616997868258372E-18, 5.318248954186068467, 6.850000000000000533 ) ) ;
#1857 = CARTESIAN_POINT ( 'NONE',  ( 1.303621121494459967, -1.237764246504700072, 6.659417683669679455 ) ) ;
#1858 = CARTESIAN_POINT ( 'NONE',  ( 2.190084968185480374, -4.032358841099290103, 3.838447030292440054 ) ) ;
#1859 = CARTESIAN_POINT ( 'NONE',  ( -1.485933537025771356, -4.796950468210009255, 3.286232459959995911 ) ) ;
#1860 = LINE ( 'NONE', #3074, #11162 ) ;
#1861 = DIRECTION ( 'NONE',  ( 3.018987445473109675E-48, 1.000000000000000000, 2.465190328815659976E-32 ) ) ;
#1862 = ORIENTED_EDGE ( 'NONE', *, *, #6717, .F. ) ;
#1863 = CARTESIAN_POINT ( 'NONE',  ( -1.869504824896970119, -0.2046610169491529518, 5.548311746956866131 ) ) ;
#1864 = CARTESIAN_POINT ( 'NONE',  ( 1.866416942370620058, -3.962493976234419790, 3.266391446483460026 ) ) ;
#1865 = ORIENTED_EDGE ( 'NONE', *, *, #11964, .F. ) ;
#1866 = EDGE_LOOP ( 'NONE', ( #12819, #6692, #5571, #10198 ) ) ;
#1867 = DIRECTION ( 'NONE',  ( -1.000000000000000000, 1.899065700016719806E-16, 0.000000000000000000 ) ) ;
#1868 = ORIENTED_EDGE ( 'NONE', *, *, #18146, .T. ) ;
#1869 = CARTESIAN_POINT ( 'NONE',  ( -0.4985810152601127254, -4.269082600342141376, 7.000035360316470445 ) ) ;
#1870 = ITEM_DEFINED_TRANSFORMATION ( 'NONE', 'NONE', #14739,  #17681 ) ;
#1871 = CARTESIAN_POINT ( 'NONE',  ( 2.043014502273419186, -5.041949152542365198, 3.006203457898239062 ) ) ;
#1872 = DIRECTION ( 'NONE',  ( 0.000000000000000000, 0.000000000000000000, 1.000000000000000000 ) ) ;
#1873 = EDGE_CURVE ( 'NONE', #14847, #15103, #9897, .T. ) ;
#1874 = CARTESIAN_POINT ( 'NONE',  ( -0.2812789908084309953, -0.4557203389830509765, 7.036533610117280624 ) ) ;
#1875 = VERTEX_POINT ( 'NONE', #5294 ) ;
#1876 = MANIFOLD_SOLID_BREP ( 'Stock-MAS-687-1', #15580 ) ;
#1877 = DIRECTION ( 'NONE',  ( -1.224646799147350002E-16, -1.000000000000000000, 0.000000000000000000 ) ) ;
#1878 = CARTESIAN_POINT ( 'NONE',  ( -2.500000000000000000, 4.700000000000000178, 1.600000000000000089 ) ) ;
#1879 = CARTESIAN_POINT ( 'NONE',  ( -1.990095963740230900, -4.847448931189385135, 5.204400533041805943 ) ) ;
#1880 = CARTESIAN_POINT ( 'NONE',  ( -1.932035991685910004, -0.5610169491525425212, 2.884370051397200818 ) ) ;
#1881 = EDGE_LOOP ( 'NONE', ( #8557, #7086, #17262, #671 ) ) ;
#1882 = PLANE ( 'NONE',  #9376 ) ;
#1883 = ADVANCED_FACE ( 'NONE', ( #15296 ), #1127, .F. ) ;
#1884 = VERTEX_POINT ( 'NONE', #8079 ) ;
#1885 = LINE ( 'NONE', #10053, #912 ) ;
#1886 = CARTESIAN_POINT ( 'NONE',  ( -2.203023580853999963, -5.542161016949149754, 3.872235369154300333 ) ) ;
#1887 = EDGE_CURVE ( 'NONE', #17150, #7174, #10459, .T. ) ;
#1888 = CARTESIAN_POINT ( 'NONE',  ( -1.899999999999999911, 9.199999999999999289, 1.600000000000000089 ) ) ;
#1889 = PRODUCT_RELATED_PRODUCT_CATEGORY ( 'part', '', ( #1066 ) ) ;
#1890 = EDGE_CURVE ( 'NONE', #3235, #13297, #10769, .T. ) ;
#1891 = CARTESIAN_POINT ( 'NONE',  ( 1.771358649600380142, -4.335106588847043696, 6.676209054601206283 ) ) ;
#1892 = ORIENTED_EDGE ( 'NONE', *, *, #340, .T. ) ;
#1893 = AXIS2_PLACEMENT_3D ( 'NONE', #5470, #12328, #11110 ) ;
#1894 = EDGE_CURVE ( 'NONE', #10460, #6927, #4075, .T. ) ;
#1895 = CARTESIAN_POINT ( 'NONE',  ( 0.5320716618284230259, -2.592325843585389755, 6.992519451207130032 ) ) ;
#1896 = EDGE_CURVE ( 'NONE', #8650, #17860, #16398, .T. ) ;
#1897 = DIRECTION ( 'NONE',  ( 0.000000000000000000, 0.000000000000000000, 1.000000000000000000 ) ) ;
#1898 = DIRECTION ( 'NONE',  ( -4.177994306516050823E-17, 0.7310552682428690385, -0.6823182503600111470 ) ) ;
#1899 = CARTESIAN_POINT ( 'NONE',  ( -0.6713553523422816083, -2.732055573315119723, 6.640150466718877098 ) ) ;
#1900 = PLANE ( 'NONE',  #6780 ) ;
#1901 = ORIENTED_EDGE ( 'NONE', *, *, #93, .T. ) ;
#1902 = DIRECTION ( 'NONE',  ( 0.000000000000000000, 1.000000000000000000, 0.000000000000000000 ) ) ;
#1903 = MANIFOLD_SOLID_BREP ( 'Stock-MAS-687-1', #1678 ) ;
#1904 = ORIENTED_EDGE ( 'NONE', *, *, #7833, .F. ) ;
#1905 = CARTESIAN_POINT ( 'NONE',  ( -1.221947981261169991, -0.5741044150835520332, 2.670403636935529956 ) ) ;
#1906 = CARTESIAN_POINT ( 'NONE',  ( 1.899999999999999911, 4.700000000000000178, 1.600000000000000089 ) ) ;
#1907 = DIRECTION ( 'NONE',  ( 0.000000000000000000, 0.000000000000000000, 1.000000000000000000 ) ) ;
#1908 = CARTESIAN_POINT ( 'NONE',  ( -1.347262683220810553, -5.175423728813555613, 6.986424775243341045 ) ) ;
#1909 = ORIENTED_EDGE ( 'NONE', *, *, #16850, .F. ) ;
#1910 = ORIENTED_EDGE ( 'NONE', *, *, #12209, .F. ) ;
#1911 = DIRECTION ( 'NONE',  ( -1.000000000000000000, 2.220446049250309876E-16, 0.000000000000000000 ) ) ;
#1912 = DIRECTION ( 'NONE',  ( 1.000000000000000000, -2.220446049250309876E-16, -6.049014748177260544E-16 ) ) ;
#1913 = EDGE_CURVE ( 'NONE', #14807, #14318, #16857, .T. ) ;
#1914 = ORIENTED_EDGE ( 'NONE', *, *, #16282, .F. ) ;
#1915 = CARTESIAN_POINT ( 'NONE',  ( 0.5134687485628864900, -2.215872354612800521, 2.096259702418241222 ) ) ;
#1916 = CARTESIAN_POINT ( 'NONE',  ( 0.9724415447670879953, -0.7068739681193980662, 2.553509270169310064 ) ) ;
#1917 = DIRECTION ( 'NONE',  ( -0.2800000000000002487, 6.217248937900899405E-17, -0.9599999999999998535 ) ) ;
#1918 = CARTESIAN_POINT ( 'NONE',  ( 2.219956784870649624, -2.173136654396199852, 3.918630970161570026 ) ) ;
#1919 = CARTESIAN_POINT ( 'NONE',  ( 0.009452110982655399438, -5.000192044704546035, 2.649999999999998579 ) ) ;
#1920 =( BOUNDED_SURFACE ( )  B_SPLINE_SURFACE ( 3, 3, ( 
 ( #428, #11716, #7201, #17444, #13288, #7644, #3648 ),
 ( #4948, #9298, #10892, #9203, #10601, #6246, #6531 ),
 ( #2382, #5139, #10700, #9406, #14867, #17802, #14667 ),
 ( #2276, #15072, #3557, #8029, #6617, #13669, #2081 ),
 ( #14965, #6426, #3371, #1985, #12095, #5235, #12275 ),
 ( #16252, #16343, #17714, #608, #981, #2182, #9016 ),
 ( #5046, #7930, #13472, #10790, #11904, #14767, #13578 ) ),
 .UNSPECIFIED., .T., .F., .F. ) 
 B_SPLINE_SURFACE_WITH_KNOTS ( ( 4, 3, 4 ),
 ( 4, 1, 1, 1, 4 ),
 ( 0.000000000000000000, 3.141592653589790007, 6.283185307179590673 ),
 ( 0.000000000000000000, 0.3003308066897660278, 0.4325493167368040237, 0.5576349185195599301, 0.7853981633974479459 ),
 .UNSPECIFIED. ) 
 GEOMETRIC_REPRESENTATION_ITEM ( )  RATIONAL_B_SPLINE_SURFACE ( (
 ( 1.000000000000000000, 1.000000000000000000, 1.000000000000000000, 1.000000000000000000, 1.000000000000000000, 1.000000000000000000, 1.000000000000000000),
 ( 0.3333333333333329818, 0.3333333333333329818, 0.3333333333333329818, 0.3333333333333329818, 0.3333333333333329818, 0.3333333333333329818, 0.3333333333333329818),
 ( 0.3333333333333329818, 0.3333333333333329818, 0.3333333333333329818, 0.3333333333333329818, 0.3333333333333329818, 0.3333333333333329818, 0.3333333333333329818),
 ( 1.000000000000000000, 1.000000000000000000, 1.000000000000000000, 1.000000000000000000, 1.000000000000000000, 1.000000000000000000, 1.000000000000000000),
 ( 0.3333333333333329818, 0.3333333333333329818, 0.3333333333333329818, 0.3333333333333329818, 0.3333333333333329818, 0.3333333333333329818, 0.3333333333333329818),
 ( 0.3333333333333329818, 0.3333333333333329818, 0.3333333333333329818, 0.3333333333333329818, 0.3333333333333329818, 0.3333333333333329818, 0.3333333333333329818),
 ( 1.000000000000000000, 1.000000000000000000, 1.000000000000000000, 1.000000000000000000, 1.000000000000000000, 1.000000000000000000, 1.000000000000000000) ) ) 
 REPRESENTATION_ITEM ( '' )  SURFACE ( )  );
#1921 = CARTESIAN_POINT ( 'NONE',  ( 2.035218756299218779, -0.8185750573155082810, 2.996768277952650106 ) ) ;
#1922 = CARTESIAN_POINT ( 'NONE',  ( -0.5921572875253809931, 3.050000000000000266, 1.600000000000000089 ) ) ;
#1923 = CARTESIAN_POINT ( 'NONE',  ( 2.331386066015260106, -0.9583047870452390260, 4.378465089518139841 ) ) ;
#1924 = B_SPLINE_CURVE_WITH_KNOTS ( 'NONE', 3,
 ( #10317, #11526, #494, #3284, #8843, #13176, #13010, #15978, #12829, #1541, #413, #11805, #332, #17428, #4747 ),
 .UNSPECIFIED., .F., .F.,
 ( 4, 1, 1, 1, 1, 1, 1, 1, 1, 1, 1, 1, 4 ),
 ( 0.000000000000000000, 0.04238384222888209873, 0.08486641011435110127, 0.1274541364341900129, 0.1700199979529180005, 0.2125927824333140037, 0.2551660849077280191, 0.2977383825900840053, 0.3403095086484199672, 0.3828788202031120358, 0.4254464832354830084, 0.4680130360808240075, 0.4999998212288440103 ),
 .UNSPECIFIED. ) ;
#1925 = FACE_OUTER_BOUND ( 'NONE', #6248, .T. ) ;
#1926 = ORIENTED_EDGE ( 'NONE', *, *, #13562, .F. ) ;
#1927 = DIRECTION ( 'NONE',  ( -1.000000000000000000, 0.000000000000000000, -6.344131569286600069E-16 ) ) ;
#1928 = ORIENTED_EDGE ( 'NONE', *, *, #5971, .F. ) ;
#1929 = CARTESIAN_POINT ( 'NONE',  ( 1.836970198721020197E-17, 3.581751045813930112, 7.700000000000000178 ) ) ;
#1930 = FACE_OUTER_BOUND ( 'NONE', #1053, .T. ) ;
#1931 = CIRCLE ( 'NONE', #9015, 1.100000000000000311 ) ;
#1932 = ADVANCED_FACE ( 'NONE', ( #16941 ), #18, .T. ) ;
#1933 = ORIENTED_EDGE ( 'NONE', *, *, #14000, .F. ) ;
#1934 = CARTESIAN_POINT ( 'NONE',  ( 0.3413183941262679655, -2.914521003261450360, 7.028571974690709823 ) ) ;
#1935 =( NAMED_UNIT ( * ) SI_UNIT ( $, .STERADIAN. ) SOLID_ANGLE_UNIT ( ) );
#1936 = DIRECTION ( 'NONE',  ( 0.000000000000000000, 0.000000000000000000, -1.000000000000000000 ) ) ;
#1937 = CARTESIAN_POINT ( 'NONE',  ( 1.699999999999999956, 2.299999999999999822, 7.599999999999999645 ) ) ;
#1938 = CARTESIAN_POINT ( 'NONE',  ( 1.480680413335799805, -1.214475958216410190, 6.529298007719799735 ) ) ;
#1939 = CARTESIAN_POINT ( 'NONE',  ( 1.567709126316360058, -3.915917399657849796, 2.944712621036570166 ) ) ;
#1940 = CARTESIAN_POINT ( 'NONE',  ( 1.727468145286579659, -3.966334852594401994, 5.809394271505055052 ) ) ;
#1941 = LINE ( 'NONE', #566, #1139 ) ;
#1942 = DIRECTION ( 'NONE',  ( 0.000000000000000000, -1.000000000000000000, 0.000000000000000000 ) ) ;
#1943 = VERTEX_POINT ( 'NONE', #4251 ) ;
#1944 = CARTESIAN_POINT ( 'NONE',  ( 0.3265524029357661506, -0.1423728813559330397, 6.726831181542982208 ) ) ;
#1945 = CARTESIAN_POINT ( 'NONE',  ( -1.630481553867809907, -3.543304787045240101, 3.002862530617889547 ) ) ;
#1946 = VERTEX_POINT ( 'NONE', #15479 ) ;
#1947 = VERTEX_POINT ( 'NONE', #12700 ) ;
#1948 = LINE ( 'NONE', #749, #16509 ) ;
#1949 = ORIENTED_EDGE ( 'NONE', *, *, #9373, .T. ) ;
#1950 = CARTESIAN_POINT ( 'NONE',  ( 2.345213174852950111, -3.803316834576379701, 4.503223853122318765 ) ) ;
#1951 = CARTESIAN_POINT ( 'NONE',  ( -2.354888465609351389, -5.202118644067803999, 5.923664702843871588 ) ) ;
#1952 = CIRCLE ( 'NONE', #8477, 0.6099999999999999867 ) ;
#1953 = DIRECTION ( 'NONE',  ( -1.000000000000000000, 1.850371707708599740E-16, 0.000000000000000000 ) ) ;
#1954 = DIRECTION ( 'NONE',  ( 0.7049180327868849183, -1.565232460946939801E-16, -0.7092887755011130224 ) ) ;
#1955 = ORIENTED_EDGE ( 'NONE', *, *, #10600, .T. ) ;
#1956 = CARTESIAN_POINT ( 'NONE',  ( -2.500000000000000000, 2.000000000000000000, 1.600000000000000089 ) ) ;
#1957 = CARTESIAN_POINT ( 'NONE',  ( -0.7854158957162378218, -3.636457940198391636, 2.803154272645148826 ) ) ;
#1958 = VECTOR ( 'NONE', #11386, 1000.000000000000000 ) ;
#1959 = CARTESIAN_POINT ( 'NONE',  ( 1.973760952634081134, -0.04004237288135625850, 2.925986839873718992 ) ) ;
#1960 = EDGE_LOOP ( 'NONE', ( #11728, #16378, #7363, #4476 ) ) ;
#1961 = AXIS2_PLACEMENT_3D ( 'NONE', #14860, #2175, #9665 ) ;
#1962 = AXIS2_PLACEMENT_3D ( 'NONE', #5821, #15388, #2971 ) ;
#1963 = CARTESIAN_POINT ( 'NONE',  ( -2.508228811380011081, -0.5091101694915260989, 5.566973598334550744 ) ) ;
#1964 = MECHANICAL_DESIGN_GEOMETRIC_PRESENTATION_REPRESENTATION (  '', ( #9672 ), #16767 ) ;
#1965 = EDGE_LOOP ( 'NONE', ( #1302, #12791, #12438, #15138 ) ) ;
#1966 = CARTESIAN_POINT ( 'NONE',  ( -0.07299321914061848715, -5.598516949152539723, 2.350000000000000089 ) ) ;
#1967 = PLANE ( 'NONE',  #2632 ) ;
#1968 = LINE ( 'NONE', #7630, #2418 ) ;
#1969 = AXIS2_PLACEMENT_3D ( 'NONE', #12920, #1350, #15714 ) ;
#1970 = CARTESIAN_POINT ( 'NONE',  ( 2.369027826908510548, -4.009070552811004440, 3.503830760997844518 ) ) ;
#1971 = ORIENTED_EDGE ( 'NONE', *, *, #8472, .T. ) ;
#1972 = CARTESIAN_POINT ( 'NONE',  ( 0.6343239990445400656, -3.500569086828630105, 2.433641963034069988 ) ) ;
#1973 = AXIS2_PLACEMENT_3D ( 'NONE', #234, #8737, #15702 ) ;
#1974 = DIRECTION ( 'NONE',  ( -5.551115123125780730E-16, -1.000000000000000000, 0.000000000000000000 ) ) ;
#1975 = VECTOR ( 'NONE', #12202, 1000.000000000000000 ) ;
#1976 = DIRECTION ( 'NONE',  ( 0.7071067811865470176, 0.000000000000000000, -0.7071067811865480168 ) ) ;
#1977 = CARTESIAN_POINT ( 'NONE',  ( -1.658519201881210714, -3.197821339080880065, 3.489952108543053377 ) ) ;
#1978 = DIRECTION ( 'NONE',  ( 0.000000000000000000, 1.000000000000000000, -1.836189155707839943E-31 ) ) ;
#1979 = CARTESIAN_POINT ( 'NONE',  ( -0.8967027089122764361, -1.195028546288099625, 6.546842195331652903 ) ) ;
#1980 = ORIENTED_EDGE ( 'NONE', *, *, #7793, .T. ) ;
#1981 = DIRECTION ( 'NONE',  ( -0.7071067811865480168, 0.7071067811865470176, 0.000000000000000000 ) ) ;
#1982 = AXIS2_PLACEMENT_3D ( 'NONE', #25, #8537, #5670 ) ;
#1983 = ADVANCED_FACE ( 'NONE', ( #1390 ), #2788, .T. ) ;
#1984 = AXIS2_PLACEMENT_3D ( 'NONE', #5604, #11249, #8735 ) ;
#1985 = CARTESIAN_POINT ( 'NONE',  ( 0.8675710780368863784, -0.4076464065212254684, 2.836323152971460981 ) ) ;
#1986 = EDGE_CURVE ( 'NONE', #3622, #12817, #17842, .T. ) ;
#1987 = ORIENTED_EDGE ( 'NONE', *, *, #6543, .T. ) ;
#1988 = CARTESIAN_POINT ( 'NONE',  ( -1.820241257191459905, -5.080331814072259533, 3.208199930689799917 ) ) ;
#1989 = CARTESIAN_POINT ( 'NONE',  ( 2.500000000000000000, 0.7500000000000000000, 7.649999999999999467 ) ) ;
#1990 = ADVANCED_FACE ( 'NONE', ( #13051 ), #7315, .F. ) ;
#1991 = DIRECTION ( 'NONE',  ( 0.000000000000000000, 6.123233995736769734E-17, -1.000000000000000000 ) ) ;
#1992 = CARTESIAN_POINT ( 'NONE',  ( -1.194742379459959869, -5.175423728813560054, 6.727584234649759409 ) ) ;
#1993 = VERTEX_POINT ( 'NONE', #5747 ) ;
#1994 = VECTOR ( 'NONE', #15620, 1000.000000000000000 ) ;
#1995 = VERTEX_POINT ( 'NONE', #4344 ) ;
#1996 = CARTESIAN_POINT ( 'NONE',  ( 0.5500000000000000444, 6.450000000000000178, 3.200000000000000178 ) ) ;
#1997 = CARTESIAN_POINT ( 'NONE',  ( -1.750000000000000000, 0.5999999999999999778, 7.599999999999999645 ) ) ;
#1998 = CARTESIAN_POINT ( 'NONE',  ( 1.307725206348619995, -0.7471169921413569615, 2.732408283416570161 ) ) ;
#1999 = VERTEX_POINT ( 'NONE', #14265 ) ;
#2000 = VECTOR ( 'NONE', #10514, 1000.000000000000000 ) ;
#2001 = CARTESIAN_POINT ( 'NONE',  ( 0.1749999999999999889, 7.700000000000000178, 1.600000000000000089 ) ) ;
#2002 = CARTESIAN_POINT ( 'NONE',  ( -1.176011442874419943, -2.052854336594789331, 2.320901267448050476 ) ) ;
#2003 = APPLICATION_CONTEXT ( 'automotive_design' ) ;
#2004 = AXIS2_PLACEMENT_3D ( 'NONE', #10840, #5097, #7983 ) ;
#2005 = CARTESIAN_POINT ( 'NONE',  ( -0.6500000000000000222, 3.050000000000000266, 2.699264068711930253 ) ) ;
#2006 = DIRECTION ( 'NONE',  ( -1.000000000000000000, 2.220446049250309876E-16, -8.269460797427580527E-16 ) ) ;
#2007 = CARTESIAN_POINT ( 'NONE',  ( -2.287919158821179799, -4.548542059801599535, 5.251517552016939483 ) ) ;
#2008 = CARTESIAN_POINT ( 'NONE',  ( 0.6536199613480476733, -5.011796459788070202, 2.109674034588110647 ) ) ;
#2009 = CIRCLE ( 'NONE', #5585, 0.09999999999999986677 ) ;
#2010 = ADVANCED_FACE ( 'NONE', ( #10010 ), #15672, .T. ) ;
#2011 = CARTESIAN_POINT ( 'NONE',  ( -1.951437470830620136, -5.057043525783970317, 3.384463041838880137 ) ) ;
#2012 = EDGE_CURVE ( 'NONE', #14546, #4205, #11057, .T. ) ;
#2013 = EDGE_CURVE ( 'NONE', #17672, #2905, #7229, .T. ) ;
#2014 = VECTOR ( 'NONE', #16436, 1000.000000000000000 ) ;
#2015 = CARTESIAN_POINT ( 'NONE',  ( 1.707817112497189926, -0.4112288135593229477, 6.319218296629480314 ) ) ;
#2016 = AXIS2_PLACEMENT_3D ( 'NONE', #11658, #8703, #8625 ) ;
#2017 = CARTESIAN_POINT ( 'NONE',  ( -1.850000000000000089, 11.25000000000000000, 7.700000000000000178 ) ) ;
#2018 = ORIENTED_EDGE ( 'NONE', *, *, #6290, .F. ) ;
#2019 = DIRECTION ( 'NONE',  ( 1.000000000000000000, 0.000000000000000000, -6.123233995736759873E-17 ) ) ;
#2020 = ORIENTED_EDGE ( 'NONE', *, *, #2963, .T. ) ;
#2021 = CARTESIAN_POINT ( 'NONE',  ( -1.000000000000000000, -7.000000000000000000, 5.700000000000000178 ) ) ;
#2022 = DIRECTION ( 'NONE',  ( 1.000000000000000000, 4.157615153618229646E-15, 0.000000000000000000 ) ) ;
#2023 = ORIENTED_EDGE ( 'NONE', *, *, #983, .F. ) ;
#2024 = ADVANCED_FACE ( 'NONE', ( #10099 ), #17114, .F. ) ;
#2025 = CARTESIAN_POINT ( 'NONE',  ( 0.1749999999999999889, 5.200000000000000178, 0.5999999999999999778 ) ) ;
#2026 = CARTESIAN_POINT ( 'NONE',  ( -0.3159454637156809409, -2.984385868126319785, 7.032150113402090064 ) ) ;
#2027 = SHAPE_REPRESENTATION ( 'Plunger Actuator', ( #17681 ), #4992 ) ;
#2028 = DIRECTION ( 'NONE',  ( 1.000000000000000000, 0.000000000000000000, 0.000000000000000000 ) ) ;
#2029 = CARTESIAN_POINT ( 'NONE',  ( -1.850000000000000089, -5.599999999999999645, 2.299999999999999822 ) ) ;
#2030 = AXIS2_PLACEMENT_3D ( 'NONE', #6738, #13497, #12015 ) ;
#2031 = LINE ( 'NONE', #13150, #5224 ) ;
#2032 = CARTESIAN_POINT ( 'NONE',  ( 0.06276132972186961034, -1.377493976234430040, 7.052616990284530374 ) ) ;
#2033 = CARTESIAN_POINT ( 'NONE',  ( -1.092567884283820012, -4.637854336594780413, 6.784476218553590066 ) ) ;
#2034 = CARTESIAN_POINT ( 'NONE',  ( -0.2475374578675481607, -4.245794312053864594, 6.738044908627027318 ) ) ;
#2035 = EDGE_CURVE ( 'NONE', #13116, #5609, #5925, .T. ) ;
#2036 = CARTESIAN_POINT ( 'NONE',  ( -1.408343819019460219E-16, 2.299999999999999822, 5.100000000000000533 ) ) ;
#2037 = DIRECTION ( 'NONE',  ( 2.220446049250309876E-16, 1.000000000000000000, 3.286920438420880041E-31 ) ) ;
#2038 = ORIENTED_EDGE ( 'NONE', *, *, #4986, .T. ) ;
#2039 = CARTESIAN_POINT ( 'NONE',  ( -1.599999999999880185, 11.40000000000000036, 1.600000000000000089 ) ) ;
#2040 = CARTESIAN_POINT ( 'NONE',  ( -0.6187874668174415671, -0.1646186440677970542, 6.657494107589526422 ) ) ;
#2041 = CARTESIAN_POINT ( 'NONE',  ( 0.3949552299394610277, -3.776187669928119828, 2.379923265530350385 ) ) ;
#2042 = VERTEX_POINT ( 'NONE', #6010 ) ;
#2043 = AXIS2_PLACEMENT_3D ( 'NONE', #13979, #15669, #1583 ) ;
#2044 = ORIENTED_EDGE ( 'NONE', *, *, #13220, .T. ) ;
#2045 = CARTESIAN_POINT ( 'NONE',  ( -1.875000000000000000, 2.220446049250309876E-16, 7.700000000000000178 ) ) ;
#2046 = ORIENTED_EDGE ( 'NONE', *, *, #4384, .T. ) ;
#2047 = PRODUCT_CONTEXT ( 'NONE', #16913, 'mechanical' ) ;
#2048 = CARTESIAN_POINT ( 'NONE',  ( -3.161120280659493168E-15, -5.600000000000000533, 2.050000000000001155 ) ) ;
#2049 = ADVANCED_FACE ( 'NONE', ( #633 ), #14529, .F. ) ;
#2050 = DIRECTION ( 'NONE',  ( -1.643460219210440021E-31, -1.000000000000000000, -2.220446049250309876E-16 ) ) ;
#2051 = DIRECTION ( 'NONE',  ( -1.000000000000000000, 0.000000000000000000, 0.000000000000000000 ) ) ;
#2052 = VERTEX_POINT ( 'NONE', #11654 ) ;
#2053 = DIRECTION ( 'NONE',  ( 3.515706244646330359E-15, -1.000000000000000000, -1.110223024625510049E-16 ) ) ;
#2054 = DIRECTION ( 'NONE',  ( -4.440892098500630106E-16, 0.000000000000000000, 1.000000000000000000 ) ) ;
#2055 = EDGE_CURVE ( 'NONE', #1463, #12743, #11934, .T. ) ;
#2056 = AXIS2_PLACEMENT_3D ( 'NONE', #3679, #17643, #9526 ) ;
#2057 = CARTESIAN_POINT ( 'NONE',  ( 0.3429245540020083860, -3.776187669928120272, 2.675820019639898906 ) ) ;
#2058 = CARTESIAN_POINT ( 'NONE',  ( -1.467041701146829746, -0.4779661016949154906, 6.911479965439912831 ) ) ;
#2059 = EDGE_CURVE ( 'NONE', #15231, #18019, #9238, .T. ) ;
#2060 = ORIENTED_EDGE ( 'NONE', *, *, #5000, .F. ) ;
#2061 = CARTESIAN_POINT ( 'NONE',  ( 0.9002849211310119948, -0.4334745762711874617, 7.196465912290821443 ) ) ;
#2062 = ORIENTED_EDGE ( 'NONE', *, *, #17684, .T. ) ;
#2063 = CARTESIAN_POINT ( 'NONE',  ( -0.4360591020458099987, -5.591101694915249887, 2.387347919655840034 ) ) ;
#2064 = EDGE_CURVE ( 'NONE', #9178, #2115, #4789, .T. ) ;
#2065 = CARTESIAN_POINT ( 'NONE',  ( 1.777964140657679382, -0.8689925102520593692, 6.241943319976220650 ) ) ;
#2066 = VECTOR ( 'NONE', #6144, 1000.000000000000000 ) ;
#2067 = CARTESIAN_POINT ( 'NONE',  ( -1.449568901432419343, -0.2625000000000002331, 3.250431098567584165 ) ) ;
#2068 = CARTESIAN_POINT ( 'NONE',  ( 0.9279264017968674727, -4.428259742000194343, 7.186376135231798301 ) ) ;
#2069 = ORIENTED_EDGE ( 'NONE', *, *, #18205, .T. ) ;
#2070 = CARTESIAN_POINT ( 'NONE',  ( 1.417709711196429856, -3.593722239981790079, 2.821478011237759986 ) ) ;
#2071 = FACE_OUTER_BOUND ( 'NONE', #22, .T. ) ;
#2072 = DIRECTION ( 'NONE',  ( -3.700743415417180054E-15, -1.000000000000000000, -2.220446049250169853E-16 ) ) ;
#2073 = CARTESIAN_POINT ( 'NONE',  ( 0.3257255101953561716, -4.175929447188994281, 6.727018681373227338 ) ) ;
#2074 = PRODUCT_DEFINITION_SHAPE ( 'NONE', 'NONE',  #18302 ) ;
#2075 = FACE_OUTER_BOUND ( 'NONE', #17568, .T. ) ;
#2076 = CARTESIAN_POINT ( 'NONE',  ( -0.03000000000000000236, 11.40000000000000036, -2.869354249208270301E-17 ) ) ;
#2077 = CARTESIAN_POINT ( 'NONE',  ( -2.044452488559148851, -1.451199717459271454, 4.887392274793804781 ) ) ;
#2078 = EDGE_LOOP ( 'NONE', ( #605, #9911, #10015, #10387 ) ) ;
#2079 = AXIS2_PLACEMENT_3D ( 'NONE', #14225, #11436, #5709 ) ;
#2080 = LINE ( 'NONE', #15070, #3772 ) ;
#2081 = CARTESIAN_POINT ( 'NONE',  ( 1.670747221194369914, -0.4963798976394459550, 3.047345349617600174 ) ) ;
#2082 = CARTESIAN_POINT ( 'NONE',  ( -0.4500319419455615089, -1.125163681423229756, 7.315451193241928607 ) ) ;
#2083 = ORIENTED_EDGE ( 'NONE', *, *, #16513, .F. ) ;
#2084 = CARTESIAN_POINT ( 'NONE',  ( 1.399999999999999911, -8.000000000000000000, 6.100000000000000533 ) ) ;
#2085 = CARTESIAN_POINT ( 'NONE',  ( -2.500000000000000000, 0.4000000000000000222, 4.000000000000000000 ) ) ;
#2086 = LINE ( 'NONE', #8117, #14209 ) ;
#2087 = EDGE_CURVE ( 'NONE', #13096, #15231, #5116, .T. ) ;
#2088 = CARTESIAN_POINT ( 'NONE',  ( 1.494593880360790550, -5.038983050847454237, 3.295456077495951153 ) ) ;
#2089 = ORIENTED_EDGE ( 'NONE', *, *, #11703, .T. ) ;
#2090 = VERTEX_POINT ( 'NONE', #4605 ) ;
#2091 = DIRECTION ( 'NONE',  ( -1.000000000000000000, 0.000000000000000000, 7.401486830834380223E-16 ) ) ;
#2092 = DIRECTION ( 'NONE',  ( 1.776356839400249824E-16, 3.552713678800500140E-16, -1.000000000000000000 ) ) ;
#2093 = CARTESIAN_POINT ( 'NONE',  ( 2.500000000000000000, 0.4000000000000000222, -2.399999999999999911 ) ) ;
#2094 = ADVANCED_FACE ( 'NONE', ( #4882 ), #4704, .T. ) ;
#2095 = EDGE_LOOP ( 'NONE', ( #12733, #15704, #149, #5080 ) ) ;
#2096 = CARTESIAN_POINT ( 'NONE',  ( 1.289141334274990447, -5.417584745762705545, 6.297747079672416426 ) ) ;
#2097 = CARTESIAN_POINT ( 'NONE',  ( 0.3578984759184136166, -2.615614131873680748, 7.329643012642057087 ) ) ;
#2098 = CARTESIAN_POINT ( 'NONE',  ( 0.1749999999999999889, 5.200000000000000178, 1.600000000000000089 ) ) ;
#2099 = CARTESIAN_POINT ( 'NONE',  ( -2.653777292528150866, -1.773394877135329839, 4.724078510415215426 ) ) ;
#2100 = FACE_OUTER_BOUND ( 'NONE', #401, .T. ) ;
#2101 = LINE ( 'NONE', #9517, #11767 ) ;
#2102 = EDGE_CURVE ( 'NONE', #620, #13315, #17647, .T. ) ;
#2103 = CARTESIAN_POINT ( 'NONE',  ( 2.345213174852950111, -3.803316834576380145, 4.503223853122319653 ) ) ;
#2104 = LINE ( 'NONE', #12118, #6711 ) ;
#2105 = CARTESIAN_POINT ( 'NONE',  ( 2.500000000000000000, 9.199999999999999289, 0.6099999999999999867 ) ) ;
#2107 = ORIENTED_EDGE ( 'NONE', *, *, #4843, .T. ) ;
#2106 = CARTESIAN_POINT ( 'NONE',  ( 0.7540633504677742849, -2.239160642901089293, 2.155495695330191364 ) ) ;
#2108 = DIRECTION ( 'NONE',  ( 0.000000000000000000, -0.2588190451025161321, 0.9659258262890695335 ) ) ;
#2109 = DIRECTION ( 'NONE',  ( 2.537652627714639929E-16, 1.000000000000000000, 0.000000000000000000 ) ) ;
#2110 = CARTESIAN_POINT ( 'NONE',  ( 1.889999999999999902, 4.100000000000000533, -6.512531667206379696E-16 ) ) ;
#2111 = CARTESIAN_POINT ( 'NONE',  ( -1.236334101859210000, -2.029566048306499670, 2.697445712080720259 ) ) ;
#2112 = CARTESIAN_POINT ( 'NONE',  ( 1.194742379459969861, -0.4245762711864409789, 6.727584234649759409 ) ) ;
#2113 = CARTESIAN_POINT ( 'NONE',  ( 0.2335786437626899970, 6.450000000000000178, 1.958578643762689753 ) ) ;
#2114 = CARTESIAN_POINT ( 'NONE',  ( 2.431060148753489081, -5.355296610169490101, 3.635668498923322112 ) ) ;
#2115 = VERTEX_POINT ( 'NONE', #2213 ) ;
#2116 = CARTESIAN_POINT ( 'NONE',  ( -1.000000000000000000, -6.000000000000000000, 5.100000000000000533 ) ) ;
#2117 = ORIENTED_EDGE ( 'NONE', *, *, #7793, .F. ) ;
#2118 = FACE_OUTER_BOUND ( 'NONE', #11604, .T. ) ;
#2119 = CARTESIAN_POINT ( 'NONE',  ( -0.9000000000000000222, 6.450000000000000178, 3.600000000000000089 ) ) ;
#2120 = EDGE_CURVE ( 'NONE', #14390, #1331, #12027, .T. ) ;
#2121 = VERTEX_POINT ( 'NONE', #2116 ) ;
#2122 = EDGE_CURVE ( 'NONE', #8619, #10260, #15928, .T. ) ;
#2123 = ORIENTED_EDGE ( 'NONE', *, *, #12897, .T. ) ;
#2124 = CARTESIAN_POINT ( 'NONE',  ( 2.301223891756920104, -2.611773255513699876, 5.193066210047949660 ) ) ;
#2125 = EDGE_CURVE ( 'NONE', #1744, #6036, #14701, .T. ) ;
#2126 = CARTESIAN_POINT ( 'NONE',  ( -0.1749999999999999889, 9.299999999999998934, 1.600000000000000089 ) ) ;
#2127 = CARTESIAN_POINT ( 'NONE',  ( 0.06264882350516240428, -5.448728813559320372, 7.052569299041220319 ) ) ;
#2128 = EDGE_CURVE ( 'NONE', #11596, #17115, #13509, .T. ) ;
#2129 = CARTESIAN_POINT ( 'NONE',  ( -1.399999999999999911, -8.000000000000000000, 3.299999999999999822 ) ) ;
#2130 = ADVANCED_FACE ( 'NONE', ( #548 ), #16192, .F. ) ;
#2131 = LINE ( 'NONE', #16031, #13550 ) ;
#2132 = EDGE_CURVE ( 'NONE', #7787, #2833, #13428, .T. ) ;
#2133 = CARTESIAN_POINT ( 'NONE',  ( -1.282210379528740063, -4.661142624883069630, 6.673494927815290190 ) ) ;
#2134 = AXIS2_PLACEMENT_3D ( 'NONE', #6282, #16388, #11942 ) ;
#2135 = CARTESIAN_POINT ( 'NONE',  ( 1.854389246811829706, -2.448755237495690462, 3.819010576716856065 ) ) ;
#2136 = CARTESIAN_POINT ( 'NONE',  ( -0.9000000000000000222, -10.00000000000000000, 6.100000000000000533 ) ) ;
#2137 = CARTESIAN_POINT ( 'NONE',  ( 1.889999999999999902, 4.700000000000000178, 0.5999999999999999778 ) ) ;
#2138 = ORIENTED_EDGE ( 'NONE', *, *, #3915, .F. ) ;
#2139 = CARTESIAN_POINT ( 'NONE',  ( -0.1749999999999999889, 9.199999999999999289, 0.4000000000000000222 ) ) ;
#2140 = CARTESIAN_POINT ( 'NONE',  ( -2.200000000000000178, 4.053507564265650114E-17, 4.000000000000000000 ) ) ;
#2141 = CARTESIAN_POINT ( 'NONE',  ( -2.283153923255329953, -3.403575057315510133, 4.129076318403500423 ) ) ;
#2142 = ORIENTED_EDGE ( 'NONE', *, *, #3124, .F. ) ;
#2143 = VECTOR ( 'NONE', #8191, 1000.000000000000000 ) ;
#2144 = ORIENTED_EDGE ( 'NONE', *, *, #15938, .F. ) ;
#2145 = CARTESIAN_POINT ( 'NONE',  ( 1.850000000000000089, -6.000000000000000000, 6.400000000000000355 ) ) ;
#2146 = SHAPE_REPRESENTATION ( 'Top Metal Cover Plate', ( #17681 ), #3818 ) ;
#2147 = VERTEX_POINT ( 'NONE', #3501 ) ;
#2148 = DIRECTION ( 'NONE',  ( 0.000000000000000000, 1.000000000000000000, 9.251858538542969116E-17 ) ) ;
#2149 = SHAPE_DEFINITION_REPRESENTATION ( #1366, #2027 ) ;
#2150 = CARTESIAN_POINT ( 'NONE',  ( 1.925796468768800063, -5.104237288135590411, 6.052706598917719560 ) ) ;
#2151 = ADVANCED_FACE ( 'NONE', ( #9145 ), #14806, .T. ) ;
#2152 = CARTESIAN_POINT ( 'NONE',  ( -1.661700935788390066, -0.5625000000000000000, 3.038299064211610112 ) ) ;
#2153 = VERTEX_POINT ( 'NONE', #9529 ) ;
#2154 = VECTOR ( 'NONE', #1976, 1000.000000000000000 ) ;
#2155 = MANIFOLD_SOLID_BREP ( 'Stock-MAS-687-1', #2859 ) ;
#2156 = VECTOR ( 'NONE', #6839, 1000.000000000000000 ) ;
#2157 = DIRECTION ( 'NONE',  ( 1.224646799147349016E-16, 0.000000000000000000, 1.000000000000000000 ) ) ;
#2158 = CARTESIAN_POINT ( 'NONE',  ( 2.018065005288410152, -4.172088570829024512, 5.077247235985069551 ) ) ;
#2159 = CARTESIAN_POINT ( 'NONE',  ( -2.043014502273419186, -0.5580508474576266753, 3.006203457898251052 ) ) ;
#2160 = EDGE_LOOP ( 'NONE', ( #17142, #2876, #13343, #1531 ) ) ;
#2161 = DIRECTION ( 'NONE',  ( 0.000000000000000000, 0.000000000000000000, -1.000000000000000000 ) ) ;
#2162 = CARTESIAN_POINT ( 'NONE',  ( 2.614198783383141045, -0.06673728813559372253, 4.243032045539284702 ) ) ;
#2163 = ORIENTED_EDGE ( 'NONE', *, *, #17084, .T. ) ;
#2164 = DIRECTION ( 'NONE',  ( 0.7071067811865470176, -0.7071067811865480168, 0.000000000000000000 ) ) ;
#2165 = CARTESIAN_POINT ( 'NONE',  ( -0.1565249325564300187, -5.453177966101690366, 7.048192310558509810 ) ) ;
#2166 = VECTOR ( 'NONE', #5635, 1000.000000000000000 ) ;
#2167 = CARTESIAN_POINT ( 'NONE',  ( 2.065623031241558660, -0.5662447625043108834, 3.572193642975259653 ) ) ;
#2168 = CARTESIAN_POINT ( 'NONE',  ( -0.4037348727536037574, -0.5906145504024216120, 2.679104755345550704 ) ) ;
#2169 = CARTESIAN_POINT ( 'NONE',  ( -1.648422021521479763, -4.684430913171365063, 6.779860219333237126 ) ) ;
#2170 = ADVANCED_FACE ( 'NONE', ( #15104 ), #15188, .F. ) ;
#2171 = ORIENTED_EDGE ( 'NONE', *, *, #7588, .T. ) ;
#2172 = PLANE ( 'NONE',  #4005 ) ;
#2173 = CARTESIAN_POINT ( 'NONE',  ( -2.276802572547989900, -3.104668185927729862, 4.104251954998810348 ) ) ;
#2174 = CYLINDRICAL_SURFACE ( 'NONE', #16153, 0.1999999999999999833 ) ;
#2175 = DIRECTION ( 'NONE',  ( 1.216682766712499758E-16, 4.229421046191059358E-17, 1.000000000000000000 ) ) ;
#2176 = CARTESIAN_POINT ( 'NONE',  ( 1.966895454505939833, -3.896469987729531681, 5.288408118292026394 ) ) ;
#2177 = DIRECTION ( 'NONE',  ( 0.000000000000000000, 0.000000000000000000, 1.000000000000000000 ) ) ;
#2178 = FACE_OUTER_BOUND ( 'NONE', #7883, .T. ) ;
#2179 = CARTESIAN_POINT ( 'NONE',  ( 2.049636678546640667, -2.243001519261071053, 4.582138519505345009 ) ) ;
#2180 = ORIENTED_EDGE ( 'NONE', *, *, #4754, .T. ) ;
#2181 = LINE ( 'NONE', #17608, #18254 ) ;
#2182 = CARTESIAN_POINT ( 'NONE',  ( 1.330034674284700458, -0.7763906680874423927, 3.132218110693851809 ) ) ;
#2183 = CARTESIAN_POINT ( 'NONE',  ( -2.653064503426820764, -3.034803321062870651, 4.766048721853594294 ) ) ;
#2184 = ORIENTED_EDGE ( 'NONE', *, *, #14180, .F. ) ;
#2185 = CARTESIAN_POINT ( 'NONE',  ( 0.1749999999999999889, 8.800000000000000711, -3.200000000000000178 ) ) ;
#2186 = CARTESIAN_POINT ( 'NONE',  ( 2.151546283159470274, -0.8884399221803740421, 3.746273477677459773 ) ) ;
#2187 = CARTESIAN_POINT ( 'NONE',  ( -1.800000000000000044, 11.29999999999999893, 1.600000000000000089 ) ) ;
#2188 = CARTESIAN_POINT ( 'NONE',  ( 2.051331987628511211, -5.073093220338980025, 4.618035453557344461 ) ) ;
#2189 = EDGE_LOOP ( 'NONE', ( #14221, #6931, #13516, #6227 ) ) ;
#2190 = ORIENTED_EDGE ( 'NONE', *, *, #1514, .T. ) ;
#2191 = EDGE_CURVE ( 'NONE', #8647, #17150, #8329, .T. ) ;
#2192 = AXIS2_PLACEMENT_3D ( 'NONE', #7153, #102, #15751 ) ;
#2193 = DIRECTION ( 'NONE',  ( 2.220446049250309876E-16, 0.000000000000000000, -1.000000000000000000 ) ) ;
#2194 = VERTEX_POINT ( 'NONE', #16656 ) ;
#2195 = CARTESIAN_POINT ( 'NONE',  ( -1.246151616534680651, -5.568855932203385706, 3.068501529594771071 ) ) ;
#2196 = CARTESIAN_POINT ( 'NONE',  ( 1.176011442874370649, -3.547145663405211646, 2.320901267448020722 ) ) ;
#2197 = CARTESIAN_POINT ( 'NONE',  ( -1.000000000000000000, -7.000000000000000000, 3.700000000000000178 ) ) ;
#2198 = CARTESIAN_POINT ( 'NONE',  ( 0.6265155281652680097, -2.891232714973161144, 7.278874170247493502 ) ) ;
#2199 = CARTESIAN_POINT ( 'NONE',  ( 1.600000000000000089, 2.886579864025409569E-16, 7.649999999999999467 ) ) ;
#2200 = CARTESIAN_POINT ( 'NONE',  ( 1.983927814618709873E-15, 10.80000000000000071, 7.700000000000000178 ) ) ;
#2201 = CARTESIAN_POINT ( 'NONE',  ( -0.4985810152601130585, -4.269082600342140488, 7.000035360316470445 ) ) ;
#2202 = DIRECTION ( 'NONE',  ( -4.476422471267237545E-17, -0.6823182503600040416, -0.7310552682428754778 ) ) ;
#2203 = DIRECTION ( 'NONE',  ( 1.000000000000000000, 0.000000000000000000, 0.000000000000000000 ) ) ;
#2205 = VERTEX_POINT ( 'NONE', #3681 ) ;
#2204 = CARTESIAN_POINT ( 'NONE',  ( -1.503451935564901643, -3.100827309567759205, 6.886949009567437052 ) ) ;
#2206 = DIRECTION ( 'NONE',  ( -3.172065784643300034E-16, 1.000000000000000000, 1.586032892321649771E-16 ) ) ;
#2207 = LINE ( 'NONE', #12020, #13126 ) ;
#2208 = CARTESIAN_POINT ( 'NONE',  ( -2.005512128484160161, -1.913124606865060029, 3.468469736471389897 ) ) ;
#2209 = CARTESIAN_POINT ( 'NONE',  ( -2.058670345754650022, -0.5491525423728820243, 3.559656372813929881 ) ) ;
#2210 = LINE ( 'NONE', #14898, #16256 ) ;
#2211 = CARTESIAN_POINT ( 'NONE',  ( -1.851073041990159984, -5.493220338983049622, 6.153284478378270528 ) ) ;
#2212 = VERTEX_POINT ( 'NONE', #1014 ) ;
#2213 = CARTESIAN_POINT ( 'NONE',  ( -0.9499999999999999556, 2.299999999999999822, 7.700000000000000178 ) ) ;
#2214 = CARTESIAN_POINT ( 'NONE',  ( 1.925796468768799397, -5.104237288135589523, 6.052706598917718672 ) ) ;
#2215 = FACE_OUTER_BOUND ( 'NONE', #14632, .T. ) ;
#2216 = CARTESIAN_POINT ( 'NONE',  ( 0.1749999999999999889, 7.900000000000000355, 0.4000000000000000222 ) ) ;
#2217 = ORIENTED_EDGE ( 'NONE', *, *, #8991, .T. ) ;
#2218 = EDGE_LOOP ( 'NONE', ( #16432, #2171, #13323, #1521 ) ) ;
#2219 = CARTESIAN_POINT ( 'NONE',  ( -2.062913653388399826, -3.217268751009200400, 5.832754583370829415 ) ) ;
#2220 = CARTESIAN_POINT ( 'NONE',  ( 0.2000000000000000111, -2.449293598294700066E-17, 8.300000000000000711 ) ) ;
#2221 = CARTESIAN_POINT ( 'NONE',  ( -1.851073041990159984, -5.493220338983049622, 6.153284478378270528 ) ) ;
#2222 = CARTESIAN_POINT ( 'NONE',  ( 1.265407828724300021, -2.309025507765960050, 2.715689360385540319 ) ) ;
#2223 = CARTESIAN_POINT ( 'NONE',  ( -1.626408692231610109, -4.707719201459649838, 6.401040991074980369 ) ) ;
#2224 = CARTESIAN_POINT ( 'NONE',  ( 1.959085573314239159, -2.635061543801990869, 5.313910057793555630 ) ) ;
#2225 = EDGE_CURVE ( 'NONE', #7642, #8282, #17855, .T. ) ;
#2226 = DIRECTION ( 'NONE',  ( 0.7071067811865480168, 0.000000000000000000, 0.7071067811865470176 ) ) ;
#2227 = PRODUCT_DEFINITION ( 'UNKNOWN', '', #1, #8436 ) ;
#2228 = CARTESIAN_POINT ( 'NONE',  ( -1.496290472746829803, -0.5672554343907050267, 2.872674968141029961 ) ) ;
#2229 = EDGE_LOOP ( 'NONE', ( #6094, #10049, #6536, #13532 ) ) ;
#2230 = EDGE_CURVE ( 'NONE', #5300, #7556, #17927, .T. ) ;
#2231 = FACE_OUTER_BOUND ( 'NONE', #2270, .T. ) ;
#2232 = LINE ( 'NONE', #13632, #3944 ) ;
#2233 = CARTESIAN_POINT ( 'NONE',  ( -2.326448859701059746, -3.380286769027220029, 4.344498395672320434 ) ) ;
#2234 = ORIENTED_EDGE ( 'NONE', *, *, #11796, .F. ) ;
#2235 = ADVANCED_FACE ( 'NONE', ( #18105 ), #11008, .T. ) ;
#2236 = ORIENTED_EDGE ( 'NONE', *, *, #9045, .T. ) ;
#2237 = EDGE_CURVE ( 'NONE', #14325, #16249, #1194, .T. ) ;
#2238 = DIRECTION ( 'NONE',  ( -7.656710514656250048E-17, 0.9659258262890690894, 0.2588190451025180749 ) ) ;
#2239 = ORIENTED_EDGE ( 'NONE', *, *, #15602, .F. ) ;
#2240 = ITEM_DEFINED_TRANSFORMATION ( 'NONE', 'NONE', #5885,  #17681 ) ;
#2241 = CARTESIAN_POINT ( 'NONE',  ( -1.851073041990159984, -5.193220338983049800, 6.153284478378270528 ) ) ;
#2242 = DIRECTION ( 'NONE',  ( -1.908195823574489776E-16, 1.000000000000000000, 0.000000000000000000 ) ) ;
#2243 = ORIENTED_EDGE ( 'NONE', *, *, #16405, .F. ) ;
#2244 = CARTESIAN_POINT ( 'NONE',  ( 1.722199153441390074, -0.5041426604022090086, 3.099360556065540173 ) ) ;
#2245 = LINE ( 'NONE', #13545, #17944 ) ;
#2246 = CARTESIAN_POINT ( 'NONE',  ( -0.03895741673419786388, -3.729611093351542284, 2.647347042895590086 ) ) ;
#2247 = CARTESIAN_POINT ( 'NONE',  ( -1.467041701146829746, -0.1779661016949160846, 6.911479965439912831 ) ) ;
#2248 = ORIENTED_EDGE ( 'NONE', *, *, #6179, .T. ) ;
#2249 = EDGE_CURVE ( 'NONE', #15397, #14568, #12147, .T. ) ;
#2250 = CARTESIAN_POINT ( 'NONE',  ( 0.9002849211310119948, -0.1334745762711869732, 7.196465912290821443 ) ) ;
#2251 = AXIS2_PLACEMENT_3D ( 'NONE', #5672, #18130, #15408 ) ;
#2252 = VERTEX_POINT ( 'NONE', #16491 ) ;
#2253 = CARTESIAN_POINT ( 'NONE',  ( -2.253200202764409799, -5.511016949152540256, 5.379408587037509903 ) ) ;
#2254 = VECTOR ( 'NONE', #5654, 1000.000000000000000 ) ;
#2255 = VECTOR ( 'NONE', #13462, 1000.000000000000000 ) ;
#2256 = CARTESIAN_POINT ( 'NONE',  ( 1.092567884283869750, -0.9621456634052130141, 6.784476218553569637 ) ) ;
#2257 = CARTESIAN_POINT ( 'NONE',  ( 2.224278379903029901, -5.390889830508481140, 5.468825643806100700 ) ) ;
#2258 = CARTESIAN_POINT ( 'NONE',  ( 1.233489123281660715, -0.9621456634052125700, 7.049812391606558037 ) ) ;
#2259 = ORIENTED_EDGE ( 'NONE', *, *, #1593, .T. ) ;
#2260 = DIRECTION ( 'NONE',  ( 0.000000000000000000, 0.000000000000000000, 1.000000000000000000 ) ) ;
#2261 = CARTESIAN_POINT ( 'NONE',  ( 1.772995665808909660, -0.8224159336754829353, 5.735078843205156041 ) ) ;
#2262 = CARTESIAN_POINT ( 'NONE',  ( -2.293791554891330353, -4.777584066324515710, 6.034778631725542297 ) ) ;
#2263 = CYLINDRICAL_SURFACE ( 'NONE', #5213, 0.8000000000000000444 ) ;
#2264 = CARTESIAN_POINT ( 'NONE',  ( 1.750000000000000000, 11.40000000000000036, 7.700000000000000178 ) ) ;
#2265 = CARTESIAN_POINT ( 'NONE',  ( -0.05638445020225820586, -4.222506023765566496, 6.752248190741917178 ) ) ;
#2266 = DIRECTION ( 'NONE',  ( 2.467162276944790449E-16, 0.000000000000000000, 1.000000000000000000 ) ) ;
#2267 = FACE_OUTER_BOUND ( 'NONE', #1262, .T. ) ;
#2268 = AXIS2_PLACEMENT_3D ( 'NONE', #15091, #9318, #7755 ) ;
#2269 = CARTESIAN_POINT ( 'NONE',  ( 2.035869680587130137, -2.289578095837640159, 4.964832940349494628 ) ) ;
#2270 = EDGE_LOOP ( 'NONE', ( #2314, #8742, #10463, #4039 ) ) ;
#2271 = CARTESIAN_POINT ( 'NONE',  ( 0.1749999999999999889, 9.500000000000000000, 3.100000000000000089 ) ) ;
#2272 = EDGE_CURVE ( 'NONE', #7510, #3530, #2337, .T. ) ;
#2273 = DIRECTION ( 'NONE',  ( -1.000000000000000000, 0.000000000000000000, 0.000000000000000000 ) ) ;
#2274 = AXIS2_PLACEMENT_3D ( 'NONE', #13510, #16289, #3503 ) ;
#2275 = EDGE_CURVE ( 'NONE', #3339, #6533, #16588, .T. ) ;
#2276 = CARTESIAN_POINT ( 'NONE',  ( 0.009452110982655408111, -0.3001920447045370310, 2.350000000000000089 ) ) ;
#2277 = CARTESIAN_POINT ( 'NONE',  ( 2.409576349373750315, -2.149848366107909303, 3.587770028483080242 ) ) ;
#2278 = ORIENTED_EDGE ( 'NONE', *, *, #11315, .F. ) ;
#2279 = CARTESIAN_POINT ( 'NONE',  ( -0.2000000000000000111, 0.1000000000000000056, 8.300000000000000711 ) ) ;
#2280 = CARTESIAN_POINT ( 'NONE',  ( 2.226511124464869873, -1.074746228486680000, 5.462491901673799610 ) ) ;
#2281 = AXIS2_PLACEMENT_3D ( 'NONE', #11073, #3857, #13858 ) ;
#2282 = CARTESIAN_POINT ( 'NONE',  ( 2.616666666666660035, -5.805074450128190455E-17, 4.000000000000000000 ) ) ;
#2283 = CARTESIAN_POINT ( 'NONE',  ( 1.795861365445541091, -5.050847457627124726, 3.705232155007893713 ) ) ;
#2284 = ORIENTED_EDGE ( 'NONE', *, *, #2467, .F. ) ;
#2285 = ORIENTED_EDGE ( 'NONE', *, *, #4500, .T. ) ;
#2286 = CARTESIAN_POINT ( 'NONE',  ( -1.889999999999999902, 3.500000000000000000, 0.5999999999999999778 ) ) ;
#2287 = CARTESIAN_POINT ( 'NONE',  ( -1.899999999999999911, 10.00000000000000000, 1.600000000000000089 ) ) ;
#2288 = DIRECTION ( 'NONE',  ( -0.000000000000000000, 1.000000000000000000, 0.000000000000000000 ) ) ;
#2289 = VERTEX_POINT ( 'NONE', #5098 ) ;
#2290 = AXIS2_PLACEMENT_3D ( 'NONE', #486, #17106, #9813 ) ;
#2291 = CARTESIAN_POINT ( 'NONE',  ( 2.143090896833110381, -5.395338983050850246, 5.672454929438339732 ) ) ;
#2292 = CIRCLE ( 'NONE', #2581, 0.2750000000000000222 ) ;
#2293 = CARTESIAN_POINT ( 'NONE',  ( -2.426866425021068974, -4.711560077819614278, 3.626019996130659617 ) ) ;
#2294 = CARTESIAN_POINT ( 'NONE',  ( 1.850000000000000089, 0.7500000000000000000, 7.700000000000000178 ) ) ;
#2295 = DIRECTION ( 'NONE',  ( 1.000000000000000000, 0.000000000000000000, 0.000000000000000000 ) ) ;
#2296 = LINE ( 'NONE', #4869, #4656 ) ;
#2297 = VECTOR ( 'NONE', #2349, 1000.000000000000000 ) ;
#2298 = CARTESIAN_POINT ( 'NONE',  ( 2.005512128484129963, -3.686875393134939394, 3.468469736471340159 ) ) ;
#2299 = CIRCLE ( 'NONE', #3766, 0.5999999999999998668 ) ;
#2300 = VECTOR ( 'NONE', #15013, 1000.000000000000114 ) ;
#2301 = LINE ( 'NONE', #6552, #12037 ) ;
#2302 = CARTESIAN_POINT ( 'NONE',  ( 1.149999999999999911, 9.274118095489749081, 7.596592582628910684 ) ) ;
#2304 = VERTEX_POINT ( 'NONE', #3612 ) ;
#2303 = CARTESIAN_POINT ( 'NONE',  ( 0.8642983280852605255, -2.867944426684881254, 7.209203477813407979 ) ) ;
#2305 = EDGE_CURVE ( 'NONE', #1710, #7550, #3894, .T. ) ;
#2306 = VECTOR ( 'NONE', #2373, 1000.000000000000000 ) ;
#2307 = PLANE ( 'NONE',  #1747 ) ;
#2308 = CARTESIAN_POINT ( 'NONE',  ( -2.234315482767910144, -0.5402542372881360411, 3.960850823455329905 ) ) ;
#2309 = VECTOR ( 'NONE', #1839, 1000.000000000000000 ) ;
#2310 = CARTESIAN_POINT ( 'NONE',  ( -0.1749999999999999889, 9.299999999999998934, 1.600000000000000089 ) ) ;
#2311 = CARTESIAN_POINT ( 'NONE',  ( -2.353343516942199898, -1.773394877135329839, 4.722803042560189901 ) ) ;
#2312 = CARTESIAN_POINT ( 'NONE',  ( -0.7093417302541390468, -0.4646186440677970153, 6.943956659919700236 ) ) ;
#2313 = DIRECTION ( 'NONE',  ( -1.000000000000000000, 0.000000000000000000, 0.000000000000000000 ) ) ;
#2314 = ORIENTED_EDGE ( 'NONE', *, *, #4250, .F. ) ;
#2315 = CARTESIAN_POINT ( 'NONE',  ( 1.791574935211219355, -5.108686440677969287, 6.226029630577610163 ) ) ;
#2316 = DIRECTION ( 'NONE',  ( 0.000000000000000000, 0.000000000000000000, 1.000000000000000000 ) ) ;
#2317 = CARTESIAN_POINT ( 'NONE',  ( 0.009452039534070141164, -0.3001931771041043140, 2.350000000173209092 ) ) ;
#2318 = COLOUR_RGB ( '', 0.09019608, 0.27058824, 0.51372549) ;
#2319 = AXIS2_PLACEMENT_3D ( 'NONE', #4785, #6269, #16097 ) ;
#2320 = ORIENTED_EDGE ( 'NONE', *, *, #10377, .T. ) ;
#2321 = CARTESIAN_POINT ( 'NONE',  ( -1.097561405233230092, -3.613169651910099756, 2.618148744692269769 ) ) ;
#2322 = VECTOR ( 'NONE', #692, 1000.000000000000000 ) ;
#2323 = CARTESIAN_POINT ( 'NONE',  ( 1.889999999999999902, 7.299999999999999822, 0.6099999999999999867 ) ) ;
#2324 = FACE_OUTER_BOUND ( 'NONE', #5273, .T. ) ;
#2325 = AXIS2_PLACEMENT_3D ( 'NONE', #13581, #9409, #13672 ) ;
#2326 = CARTESIAN_POINT ( 'NONE',  ( -1.850000000000000089, 11.25000000000000000, 7.649999999999999467 ) ) ;
#2327 = CARTESIAN_POINT ( 'NONE',  ( 0.1226612266411070129, -2.937809291549740021, 7.050255286338659388 ) ) ;
#2328 = VECTOR ( 'NONE', #2206, 1000.000000000000000 ) ;
#2329 = CARTESIAN_POINT ( 'NONE',  ( -0.8092638295168711471, -4.911779243796850380, 2.486823565593870189 ) ) ;
#2330 = AXIS2_PLACEMENT_3D ( 'NONE', #16469, #5372, #3784 ) ;
#2331 = CARTESIAN_POINT ( 'NONE',  ( -1.727468145286550127, -1.633665147405598761, 5.809394271505101237 ) ) ;
#2332 = CARTESIAN_POINT ( 'NONE',  ( -1.300961508564169922, -0.4779661016949160457, 6.661123742937279602 ) ) ;
#2333 = CARTESIAN_POINT ( 'NONE',  ( -1.899999999999999911, 2.799999999999999822, 1.600000000000000089 ) ) ;
#2334 = CARTESIAN_POINT ( 'NONE',  ( -1.661700935788390066, -0.2625000000000000111, 3.038299064211610112 ) ) ;
#2335 = VERTEX_POINT ( 'NONE', #16397 ) ;
#2336 = AXIS2_PLACEMENT_3D ( 'NONE', #13345, #3420, #15961 ) ;
#2337 = LINE ( 'NONE', #6581, #17545 ) ;
#2338 = SURFACE_SIDE_STYLE ('',( #13981 ) ) ;
#2339 = EDGE_LOOP ( 'NONE', ( #13552, #7058, #6337, #8230 ) ) ;
#2340 = ORIENTED_EDGE ( 'NONE', *, *, #14430, .F. ) ;
#2341 = VERTEX_POINT ( 'NONE', #3700 ) ;
#2342 = CARTESIAN_POINT ( 'NONE',  ( 0.5999999999999999778, 10.80000000000000071, 7.599999999999999645 ) ) ;
#2343 = AXIS2_PLACEMENT_3D ( 'NONE', #9293, #7922, #5134 ) ;
#2344 = CARTESIAN_POINT ( 'NONE',  ( -2.253200202764409799, -5.211016949152540434, 5.379408587037509903 ) ) ;
#2345 = VECTOR ( 'NONE', #6024, 1000.000000000000000 ) ;
#2346 = ORIENTED_EDGE ( 'NONE', *, *, #7368, .T. ) ;
#2347 = CARTESIAN_POINT ( 'NONE',  ( -2.311987889326990064, -1.521064582324129999, 4.260161748947139948 ) ) ;
#2348 = EDGE_CURVE ( 'NONE', #8437, #4854, #10552, .T. ) ;
#2349 = DIRECTION ( 'NONE',  ( 1.000000000000000000, 0.000000000000000000, 0.000000000000000000 ) ) ;
#2350 = EDGE_CURVE ( 'NONE', #10455, #2720, #16306, .T. ) ;
#2351 = CARTESIAN_POINT ( 'NONE',  ( -2.049150047780149642, -4.894025507765944916, 4.826039376028564476 ) ) ;
#2352 = CARTESIAN_POINT ( 'NONE',  ( 1.549742865090599997, -0.1156779661016950067, 6.471102547561449647 ) ) ;
#2353 = EDGE_LOOP ( 'NONE', ( #7227, #106, #15475, #17569 ) ) ;
#2354 = CARTESIAN_POINT ( 'NONE',  ( 1.438959988998139914E-16, -0.2999999999999999889, 2.350000000000000089 ) ) ;
#2355 = AXIS2_PLACEMENT_3D ( 'NONE', #12983, #1861, #6115 ) ;
#2356 = CARTESIAN_POINT ( 'NONE',  ( 0.6640878839024751956, -0.1379237288135599648, 7.269405042592523181 ) ) ;
#2357 = ORIENTED_EDGE ( 'NONE', *, *, #17305, .T. ) ;
#2358 = DIRECTION ( 'NONE',  ( 0.000000000000000000, 0.000000000000000000, 1.000000000000000000 ) ) ;
#2359 = CARTESIAN_POINT ( 'NONE',  ( -2.102728310581289062, -1.358046564306110593, 5.757014351541100083 ) ) ;
#2360 = CARTESIAN_POINT ( 'NONE',  ( -1.000896394980330006, -5.470974576271190770, 6.829956240957379521 ) ) ;
#2361 = CARTESIAN_POINT ( 'NONE',  ( -0.4500319419455615089, -1.125163681423229756, 7.315451193241928607 ) ) ;
#2362 = ORIENTED_EDGE ( 'NONE', *, *, #1843, .T. ) ;
#2363 = EDGE_CURVE ( 'NONE', #13435, #17446, #9548, .T. ) ;
#2364 = DIRECTION ( 'NONE',  ( -0.7071067811865480168, 0.000000000000000000, -0.7071067811865470176 ) ) ;
#2365 = VECTOR ( 'NONE', #14263, 1000.000000000000000 ) ;
#2366 = CARTESIAN_POINT ( 'NONE',  ( -2.151546283159490258, -4.711560077819619607, 3.746273477677509955 ) ) ;
#2367 = EDGE_CURVE ( 'NONE', #6950, #8261, #14827, .T. ) ;
#2368 = CARTESIAN_POINT ( 'NONE',  ( 1.947945325730759292, -4.311818300558746486, 6.502393603230323116 ) ) ;
#2369 = EDGE_CURVE ( 'NONE', #13468, #7602, #7784, .T. ) ;
#2370 = DIRECTION ( 'NONE',  ( 0.000000000000000000, -1.000000000000000000, 0.000000000000000000 ) ) ;
#2371 = EDGE_CURVE ( 'NONE', #6313, #3213, #6671, .T. ) ;
#2372 = CARTESIAN_POINT ( 'NONE',  ( -2.045969882616350155, -1.796683165423619055, 4.529973290172065070 ) ) ;
#2373 = DIRECTION ( 'NONE',  ( 0.000000000000000000, 1.000000000000000000, -1.586032892321649771E-16 ) ) ;
#2374 = CARTESIAN_POINT ( 'NONE',  ( 1.800000000000000044, 11.40000000000000036, 7.649999999999999467 ) ) ;
#2375 = CARTESIAN_POINT ( 'NONE',  ( 1.698651900122530867, -2.406019537279079579, 5.853032334688926142 ) ) ;
#2376 = VERTEX_POINT ( 'NONE', #10661 ) ;
#2377 = PLANE ( 'NONE',  #12009 ) ;
#2378 = CARTESIAN_POINT ( 'NONE',  ( -1.399999999999999911, 0.5999999999999999778, 6.100000000000000533 ) ) ;
#2379 = EDGE_CURVE ( 'NONE', #16402, #8925, #745, .T. ) ;
#2380 = CARTESIAN_POINT ( 'NONE',  ( -0.6187874668174415671, -0.1646186440677970542, 6.657494107589526422 ) ) ;
#2381 = APPLICATION_CONTEXT ( 'automotive_design' ) ;
#2382 = CARTESIAN_POINT ( 'NONE',  ( 0.009452110982655399438, -0.3001920447045380858, 2.050000000000001155 ) ) ;
#2383 = CARTESIAN_POINT ( 'NONE',  ( 0.2938780505771511620, -1.893677194936738806, 2.062434951628520086 ) ) ;
#2384 = ORIENTED_EDGE ( 'NONE', *, *, #10846, .T. ) ;
#2385 = AXIS2_PLACEMENT_3D ( 'NONE', #14120, #14223, #8573 ) ;
#2386 = CARTESIAN_POINT ( 'NONE',  ( 0.3750000000000000000, 6.450000000000000178, 2.100000000000000089 ) ) ;
#2387 = CARTESIAN_POINT ( 'NONE',  ( -0.8298945877350979439, -5.211074464177370302, 2.494426474263899962 ) ) ;
#2388 = CARTESIAN_POINT ( 'NONE',  ( 0.9150601050661639757, -5.130932203389829915, 6.868218666554230190 ) ) ;
#2389 = ORIENTED_EDGE ( 'NONE', *, *, #5298, .F. ) ;
#2390 = VERTEX_POINT ( 'NONE', #14921 ) ;
#2391 = DIRECTION ( 'NONE',  ( 0.000000000000000000, -1.000000000000000000, 0.000000000000000000 ) ) ;
#2392 = DIRECTION ( 'NONE',  ( -0.7071067811865489050, 0.000000000000000000, 0.7071067811865461294 ) ) ;
#2393 = CARTESIAN_POINT ( 'NONE',  ( -1.899999999999999911, 2.000000000000000000, 1.600000000000000089 ) ) ;
#2394 = ORIENTED_EDGE ( 'NONE', *, *, #13617, .T. ) ;
#2395 = CARTESIAN_POINT ( 'NONE',  ( 1.811729841638690219, -5.341949152542369461, 3.197954009834290012 ) ) ;
#2396 = CARTESIAN_POINT ( 'NONE',  ( 2.260671505268459391, -3.686875393134939394, 3.309864021662241029 ) ) ;
#2397 = CARTESIAN_POINT ( 'NONE',  ( 0.5500000000000000444, 3.050000000000000266, 2.699264068711930253 ) ) ;
#2398 = CARTESIAN_POINT ( 'NONE',  ( -2.623186471072040504, -3.380286769027221805, 4.297499775172091141 ) ) ;
#2399 = ADVANCED_FACE ( 'NONE', ( #12327 ), #17853, .F. ) ;
#2400 = CARTESIAN_POINT ( 'NONE',  ( -0.5500000000000000444, 0.5999999999999999778, 3.299999999999999822 ) ) ;
#2401 = VECTOR ( 'NONE', #5025, 1000.000000000000000 ) ;
#2402 = CARTESIAN_POINT ( 'NONE',  ( -0.01716182025094739952, -3.430704221963770006, 2.346608583467349796 ) ) ;
#2403 = CARTESIAN_POINT ( 'NONE',  ( 1.550000000000000044, -5.599999999999999645, 5.100000000000000533 ) ) ;
#2404 = CARTESIAN_POINT ( 'NONE',  ( 2.500000000000000000, 2.000000000000000000, 0.5999999999999999778 ) ) ;
#2406 = ORIENTED_EDGE ( 'NONE', *, *, #15210, .F. ) ;
#2405 = CARTESIAN_POINT ( 'NONE',  ( 0.6265155281652680097, -2.891232714973161144, 7.278874170247493502 ) ) ;
#2407 = CARTESIAN_POINT ( 'NONE',  ( -1.850000000000000089, -5.599999999999999645, 6.400000000000000355 ) ) ;
#2408 = CARTESIAN_POINT ( 'NONE',  ( 2.011500846714319835, -0.3489406779661020086, 3.478373409938460448 ) ) ;
#2409 = CARTESIAN_POINT ( 'NONE',  ( 1.303621121494459967, -1.237764246504700072, 6.659417683669679455 ) ) ;
#2410 = CARTESIAN_POINT ( 'NONE',  ( -2.328217775191430139, -0.5180084745762719711, 5.043379051721170292 ) ) ;
#2411 = CARTESIAN_POINT ( 'NONE',  ( 1.000000000000000000, -6.000000000000000000, 5.100000000000000533 ) ) ;
#2412 = CARTESIAN_POINT ( 'NONE',  ( -0.07299321914061848715, -5.598516949152539723, 2.350000000000000089 ) ) ;
#2413 = VERTEX_POINT ( 'NONE', #7984 ) ;
#2414 = EDGE_CURVE ( 'NONE', #11896, #13928, #2232, .T. ) ;
#2415 = VERTEX_POINT ( 'NONE', #7878 ) ;
#2416 = CARTESIAN_POINT ( 'NONE',  ( -0.7983658734557951275, -5.166525423728808519, 6.913847129767330735 ) ) ;
#2417 = PLANE ( 'NONE',  #9639 ) ;
#2418 = VECTOR ( 'NONE', #594, 1000.000000000000000 ) ;
#2419 = FACE_OUTER_BOUND ( 'NONE', #5055, .T. ) ;
#2420 = EDGE_LOOP ( 'NONE', ( #15992, #15997, #13998, #17452 ) ) ;
#2421 = CARTESIAN_POINT ( 'NONE',  ( -2.219956784870669608, -3.426863345603790023, 3.918630970161619764 ) ) ;
#2422 = ADVANCED_FACE ( 'NONE', ( #15020 ), #12235, .T. ) ;
#2423 = LINE ( 'NONE', #3790, #255 ) ;
#2424 = CARTESIAN_POINT ( 'NONE',  ( -1.428515267734880023, -5.568855932203390147, 2.829745655876930055 ) ) ;
#2425 = DIRECTION ( 'NONE',  ( 2.960594732333750117E-16, -1.000000000000000000, 0.000000000000000000 ) ) ;
#2426 = PLANE ( 'NONE',  #11432 ) ;
#2427 = CARTESIAN_POINT ( 'NONE',  ( -2.199335452462570117, -1.866548030288480042, 3.862342996790939953 ) ) ;
#2428 = CARTESIAN_POINT ( 'NONE',  ( -2.334748642087669523, -4.940602084342530453, 4.403867486184871005 ) ) ;
#2429 = CARTESIAN_POINT ( 'NONE',  ( -2.013199450439951299, -1.726818300558751851, 5.102405038955014405 ) ) ;
#2430 = DIRECTION ( 'NONE',  ( -2.775557561562890365E-16, -1.000000000000000000, -2.775557561562890365E-16 ) ) ;
#2431 = CARTESIAN_POINT ( 'NONE',  ( -1.303682947472720954, -0.2673043920988010802, 3.104350467804975366 ) ) ;
#2432 = ORIENTED_EDGE ( 'NONE', *, *, #18096, .F. ) ;
#2433 = LINE ( 'NONE', #8078, #16668 ) ;
#2434 = CARTESIAN_POINT ( 'NONE',  ( -0.03714311608457869507, -4.521412895153340550, 7.053160869216429596 ) ) ;
#2435 = EDGE_LOOP ( 'NONE', ( #14296, #16546, #16833, #9896 ) ) ;
#2436 = VERTEX_POINT ( 'NONE', #5192 ) ;
#2437 = VERTEX_POINT ( 'NONE', #6771 ) ;
#2438 = CARTESIAN_POINT ( 'NONE',  ( -0.6500000000000000222, 3.050000000000000266, 2.699264068711930253 ) ) ;
#2439 = CARTESIAN_POINT ( 'NONE',  ( -2.011500846714319835, -5.251059322033900578, 3.478373409938470218 ) ) ;
#2440 = DIRECTION ( 'NONE',  ( 0.000000000000000000, 0.000000000000000000, 1.000000000000000000 ) ) ;
#2441 = CARTESIAN_POINT ( 'NONE',  ( -2.516451517878150135, -4.688271789531334832, 3.857037693030694214 ) ) ;
#2442 = CARTESIAN_POINT ( 'NONE',  ( -2.500000000000000000, 9.199999999999999289, 1.600000000000000089 ) ) ;
#2443 = CARTESIAN_POINT ( 'NONE',  ( 0.4985810152601650724, -1.330917399657850053, 7.000035360316460675 ) ) ;
#2444 = VECTOR ( 'NONE', #2629, 1000.000000000000000 ) ;
#2445 = CARTESIAN_POINT ( 'NONE',  ( 2.318251751302029984, -0.06673728813559359763, 4.294764266798990704 ) ) ;
#2446 = ORIENTED_EDGE ( 'NONE', *, *, #17628, .T. ) ;
#2447 = CARTESIAN_POINT ( 'NONE',  ( -1.791574935211209807, -0.4913135593220339659, 6.226029630577610163 ) ) ;
#2448 = VERTEX_POINT ( 'NONE', #10842 ) ;
#2449 = CARTESIAN_POINT ( 'NONE',  ( -2.043014502273419186, -0.2580508474576271305, 3.006203457898251052 ) ) ;
#2450 = CARTESIAN_POINT ( 'NONE',  ( -0.2000000000000000111, 2.449293598294710235E-17, 8.300000000000000711 ) ) ;
#2451 = CARTESIAN_POINT ( 'NONE',  ( 1.951437470830589271, -0.5429564742160231106, 3.384463041838830843 ) ) ;
#2452 = EDGE_CURVE ( 'NONE', #17576, #3272, #2433, .T. ) ;
#2453 = CARTESIAN_POINT ( 'NONE',  ( -2.270487904532170198, -5.537711864406779760, 4.080813552109679776 ) ) ;
#2454 = CARTESIAN_POINT ( 'NONE',  ( 1.940935473245969156, -0.5041426604022095637, 2.893832807158179143 ) ) ;
#2455 = VERTEX_POINT ( 'NONE', #10943 ) ;
#2456 = PLANE ( 'NONE',  #7861 ) ;
#2457 = VECTOR ( 'NONE', #17273, 1000.000000000000000 ) ;
#2458 = CARTESIAN_POINT ( 'NONE',  ( 0.8001898266890951072, -4.129352870612410520, 6.913242401714550844 ) ) ;
#2459 = CARTESIAN_POINT ( 'NONE',  ( -2.589817782457070727, -4.963890372630814340, 4.120381550730010112 ) ) ;
#2460 = DIRECTION ( 'NONE',  ( -1.306144734853129823E-16, -6.530723674265629391E-17, 1.000000000000000000 ) ) ;
#2461 = LINE ( 'NONE', #13744, #2914 ) ;
#2462 = CARTESIAN_POINT ( 'NONE',  ( 1.785776242921180756, -1.121322805063259542, 5.712869711683790541 ) ) ;
#2463 = LINE ( 'NONE', #5226, #13825 ) ;
#2464 = ORIENTED_EDGE ( 'NONE', *, *, #7104, .T. ) ;
#2465 = CARTESIAN_POINT ( 'NONE',  ( 2.241103642439659443E-15, 9.099999999999999645, 7.700000000000000178 ) ) ;
#2466 = CARTESIAN_POINT ( 'NONE',  ( 2.500000000000000000, 9.199999999999999289, 1.600000000000000089 ) ) ;
#2467 = EDGE_CURVE ( 'NONE', #16167, #4320, #12419, .T. ) ;
#2468 = CARTESIAN_POINT ( 'NONE',  ( -2.567863625471609179, -3.104668185927728974, 4.029783546918099368 ) ) ;
#2469 = DIRECTION ( 'NONE',  ( -1.224646799147351975E-16, 1.000000000000000000, 6.123233995736750012E-17 ) ) ;
#2470 = PRODUCT_RELATED_PRODUCT_CATEGORY ( 'part', '', ( #13935 ) ) ;
#2471 = DIRECTION ( 'NONE',  ( 1.853875224168160112E-15, 1.000000000000000000, 2.960594732333760372E-15 ) ) ;
#2472 = CARTESIAN_POINT ( 'NONE',  ( 2.050059171113549183, -5.377542372881360500, 4.809263467226075228 ) ) ;
#2473 = ORIENTED_EDGE ( 'NONE', *, *, #9614, .T. ) ;
#2474 = EDGE_CURVE ( 'NONE', #7262, #6008, #18211, .T. ) ;
#2475 = DIRECTION ( 'NONE',  ( -2.400482215405740060E-16, 0.000000000000000000, 1.000000000000000000 ) ) ;
#2476 = ADVANCED_FACE ( 'NONE', ( #5662 ), #16757, .F. ) ;
#2477 = CARTESIAN_POINT ( 'NONE',  ( -1.899999999999999911, 4.700000000000000178, 0.6099999999999999867 ) ) ;
#2478 = PLANE ( 'NONE',  #6394 ) ;
#2479 = EDGE_CURVE ( 'NONE', #14900, #412, #14006, .T. ) ;
#2480 = EDGE_LOOP ( 'NONE', ( #6075, #9587, #4860, #5883 ) ) ;
#2481 = CARTESIAN_POINT ( 'NONE',  ( -1.596341326794979976, -5.564406779661021041, 2.970780074643819990 ) ) ;
#2482 = CARTESIAN_POINT ( 'NONE',  ( 1.558664967382918931, -4.059488005747546424, 6.847947208954417775 ) ) ;
#2483 = CARTESIAN_POINT ( 'NONE',  ( 0.4469859058769135030, -3.776187669928120272, 2.084026511420788985 ) ) ;
#2484 = DIRECTION ( 'NONE',  ( 0.000000000000000000, -1.000000000000000000, 0.000000000000000000 ) ) ;
#2485 = CARTESIAN_POINT ( 'NONE',  ( -2.291237445532080308, -4.664983501243040287, 4.162434510291849854 ) ) ;
#2486 = DIRECTION ( 'NONE',  ( 0.000000000000000000, -0.4472135954999567065, -0.8944271909999164105 ) ) ;
#2487 = DIRECTION ( 'NONE',  ( 1.000000000000000000, 0.000000000000000000, 0.000000000000000000 ) ) ;
#2488 = ORIENTED_EDGE ( 'NONE', *, *, #760, .T. ) ;
#2489 = CARTESIAN_POINT ( 'NONE',  ( 0.1749999999999999889, 7.700000000000000178, 1.600000000000000089 ) ) ;
#2490 = CARTESIAN_POINT ( 'NONE',  ( 2.088297318559229954, -0.3978813559322040283, 5.785136623276629919 ) ) ;
#2491 = CARTESIAN_POINT ( 'NONE',  ( -1.586727176531439909, -1.982989471729919906, 2.961885344765640138 ) ) ;
#2492 = CARTESIAN_POINT ( 'NONE',  ( -0.9000000000000000222, 2.050000000000000266, 1.600000000000000089 ) ) ;
#2493 = LINE ( 'NONE', #1011, #11245 ) ;
#2494 = CARTESIAN_POINT ( 'NONE',  ( -2.268288188848061715, -5.551059322033894183, 3.322421079292323665 ) ) ;
#2495 = ORIENTED_EDGE ( 'NONE', *, *, #5541, .T. ) ;
#2496 = ADVANCED_FACE ( 'NONE', ( #1496 ), #7228, .F. ) ;
#2497 =( LENGTH_UNIT ( ) NAMED_UNIT ( * ) SI_UNIT ( .MILLI., .METRE. ) );
#2498 = CARTESIAN_POINT ( 'NONE',  ( 2.293398556041700065, -5.064194915254238261, 4.171956209133471205 ) ) ;
#2499 = DIRECTION ( 'NONE',  ( -0.7071067811865475727, -0.7071067811865475727, 0.000000000000000000 ) ) ;
#2500 = DIRECTION ( 'NONE',  ( 1.000000000000000000, -1.608122649676639805E-16, 0.000000000000000000 ) ) ;
#2501 = ORIENTED_EDGE ( 'NONE', *, *, #9432, .T. ) ;
#2502 = CARTESIAN_POINT ( 'NONE',  ( 2.313035575219750228, -4.172088570829020071, 5.134294963419709923 ) ) ;
#2503 = PLANE ( 'NONE',  #4069 ) ;
#2504 = CARTESIAN_POINT ( 'NONE',  ( -2.203023580853999963, -5.542161016949149754, 3.872235369154300333 ) ) ;
#2505 = CARTESIAN_POINT ( 'NONE',  ( -1.850000000000000089, -5.599999999999999645, 2.799999999999999822 ) ) ;
#2506 = CARTESIAN_POINT ( 'NONE',  ( -2.237394498046660019, -3.263845327585780165, 5.429939413646380331 ) ) ;
#2507 = CARTESIAN_POINT ( 'NONE',  ( 1.889999999999999902, 7.900000000000000355, 2.872493252184739990E-16 ) ) ;
#2508 = CARTESIAN_POINT ( 'NONE',  ( -1.842787987253248883, -1.889836318576769036, 3.794994874786233652 ) ) ;
#2509 = CARTESIAN_POINT ( 'NONE',  ( 1.899999999999999911, 0.5999999999999999778, 7.599999999999999645 ) ) ;
#2510 = FACE_OUTER_BOUND ( 'NONE', #10800, .T. ) ;
#2511 = ORIENTED_EDGE ( 'NONE', *, *, #14365, .F. ) ;
#2512 = ADVANCED_FACE ( 'NONE', ( #16188 ), #14895, .T. ) ;
#2513 = DIRECTION ( 'NONE',  ( -2.220446049250309876E-16, 0.000000000000000000, -1.000000000000000000 ) ) ;
#2514 = CARTESIAN_POINT ( 'NONE',  ( -1.777964140657649850, -4.731007489747940831, 6.241943319976260618 ) ) ;
#2515 = VERTEX_POINT ( 'NONE', #7959 ) ;
#2516 = EDGE_LOOP ( 'NONE', ( #12505, #3361, #3055, #8702 ) ) ;
#2517 = UNCERTAINTY_MEASURE_WITH_UNIT (LENGTH_MEASURE( 1.000000000000000082E-05 ), #4504, 'distance_accuracy_value', 'NONE');
#2518 = ORIENTED_EDGE ( 'NONE', *, *, #16251, .F. ) ;
#2519 = LINE ( 'NONE', #18218, #5371 ) ;
#2520 = CARTESIAN_POINT ( 'NONE',  ( -0.4360591020458099987, -5.291101694915250064, 2.387347919655840034 ) ) ;
#2521 = CIRCLE ( 'NONE', #15240, 0.1999999999999999833 ) ;
#2522 = ORIENTED_EDGE ( 'NONE', *, *, #4732, .F. ) ;
#2523 = CARTESIAN_POINT ( 'NONE',  ( 2.065623031241559548, -0.5662447625043109944, 3.572193642975259653 ) ) ;
#2524 = CARTESIAN_POINT ( 'NONE',  ( 1.149999999999999911, 9.299999999999998934, 7.500000000000000000 ) ) ;
#2525 = CARTESIAN_POINT ( 'NONE',  ( -2.182690844914350059, -1.680241723982170088, 5.580117243900479806 ) ) ;
#2526 = CARTESIAN_POINT ( 'NONE',  ( 0.4221287159901364605, -0.1423728813559330397, 7.320050063945812369 ) ) ;
#2527 = CARTESIAN_POINT ( 'NONE',  ( -2.043308330018790198, -0.5002118644067800046, 5.867646457774669422 ) ) ;
#2528 = ORIENTED_EDGE ( 'NONE', *, *, #1332, .T. ) ;
#2529 = CARTESIAN_POINT ( 'NONE',  ( 1.750316316486830059, -0.04004237288135630013, 3.126818518378580158 ) ) ;
#2530 = ORIENTED_EDGE ( 'NONE', *, *, #2237, .F. ) ;
#2531 = CARTESIAN_POINT ( 'NONE',  ( 0.4000000000000000222, 2.399999999999999911, 6.100000000000000533 ) ) ;
#2532 = CARTESIAN_POINT ( 'NONE',  ( 0.5320716618284228039, -2.592325843585389311, 6.992519451207130032 ) ) ;
#2533 = CARTESIAN_POINT ( 'NONE',  ( -2.306642602145299925, -5.515466101694909362, 5.166805192608490138 ) ) ;
#2534 = CARTESIAN_POINT ( 'NONE',  ( -1.835211330903778970, -4.707719201459645397, 6.617058440404012032 ) ) ;
#2535 = ORIENTED_EDGE ( 'NONE', *, *, #2695, .F. ) ;
#2536 = CARTESIAN_POINT ( 'NONE',  ( 0.000000000000000000, 0.000000000000000000, 5.100000000000000533 ) ) ;
#2537 = CARTESIAN_POINT ( 'NONE',  ( 0.1569242594330760021, -4.199217735477280833, 7.048216443236290374 ) ) ;
#2538 = FACE_OUTER_BOUND ( 'NONE', #14728, .T. ) ;
#2539 = CARTESIAN_POINT ( 'NONE',  ( 0.9000000000000000222, 2.050000000000000266, 3.600000000000000089 ) ) ;
#2540 = LINE ( 'NONE', #12455, #14185 ) ;
#2541 = CARTESIAN_POINT ( 'NONE',  ( -1.043047520545169471, -1.517223705964159786, 6.468319459971155538 ) ) ;
#2542 = DIRECTION ( 'NONE',  ( 0.000000000000000000, 0.000000000000000000, 1.000000000000000000 ) ) ;
#2543 = ORIENTED_EDGE ( 'NONE', *, *, #6066, .F. ) ;
#2544 = FACE_OUTER_BOUND ( 'NONE', #16780, .T. ) ;
#2545 = DIRECTION ( 'NONE',  ( -1.000000000000000000, 0.000000000000000000, 0.000000000000000000 ) ) ;
#2546 = CARTESIAN_POINT ( 'NONE',  ( -1.562863241354461641, -0.1913135593220339215, 6.031217337312382298 ) ) ;
#2547 = AXIS2_PLACEMENT_3D ( 'NONE', #17886, #15337, #3732 ) ;
#2548 = AXIS2_PLACEMENT_3D ( 'NONE', #5823, #12864, #7222 ) ;
#2549 = CARTESIAN_POINT ( 'NONE',  ( -0.4469859058769716786, -1.823812330071880705, 2.084026511420800976 ) ) ;
#2550 = ORIENTED_EDGE ( 'NONE', *, *, #16540, .F. ) ;
#2551 = VECTOR ( 'NONE', #6022, 1000.000000000000000 ) ;
#2552 = CARTESIAN_POINT ( 'NONE',  ( -0.4446501070882830087, -4.952022267818760426, 2.379695998155090031 ) ) ;
#2553 = CARTESIAN_POINT ( 'NONE',  ( -1.921786527979019166, -5.242161016949150820, 3.977907449687794195 ) ) ;
#2554 = ORIENTED_EDGE ( 'NONE', *, *, #12443, .T. ) ;
#2555 = FACE_OUTER_BOUND ( 'NONE', #7880, .T. ) ;
#2556 = DIRECTION ( 'NONE',  ( 6.123233995736767268E-17, 1.000000000000000000, 0.000000000000000000 ) ) ;
#2557 = CARTESIAN_POINT ( 'NONE',  ( -2.500000000000000000, 10.00000000000000000, 1.600000000000000089 ) ) ;
#2558 = EDGE_LOOP ( 'NONE', ( #724, #14028, #6116, #7517 ) ) ;
#2559 = CARTESIAN_POINT ( 'NONE',  ( -0.1565249325564300187, -5.453177966101690366, 7.048192310558509810 ) ) ;
#2560 = CARTESIAN_POINT ( 'NONE',  ( 1.132648842710480830, -4.106064582324130185, 7.100045893750476900 ) ) ;
#2561 = CARTESIAN_POINT ( 'NONE',  ( 2.247144151254821143, -3.985782264522713447, 3.288101683376901452 ) ) ;
#2562 = CIRCLE ( 'NONE', #784, 0.1000000000000002554 ) ;
#2563 = LINE ( 'NONE', #13764, #6730 ) ;
#2564 = CARTESIAN_POINT ( 'NONE',  ( -1.065036425887979421, -1.218316834576379737, 6.455163597548632559 ) ) ;
#2565 = EDGE_CURVE ( 'NONE', #12747, #14464, #14696, .T. ) ;
#2566 = DIRECTION ( 'NONE',  ( 1.000000000000000000, 9.280995951607650285E-16, 0.000000000000000000 ) ) ;
#2567 = LINE ( 'NONE', #16456, #17986 ) ;
#2568 = VERTEX_POINT ( 'NONE', #9434 ) ;
#2569 = EDGE_CURVE ( 'NONE', #8663, #9757, #2207, .T. ) ;
#2570 = VECTOR ( 'NONE', #3019, 1000.000000000000000 ) ;
#2571 = EDGE_CURVE ( 'NONE', #1999, #14325, #12931, .T. ) ;
#2572 = LINE ( 'NONE', #4225, #17380 ) ;
#2573 = CARTESIAN_POINT ( 'NONE',  ( 2.614198783383141045, -0.3667372881355940861, 4.243032045539284702 ) ) ;
#2574 = CARTESIAN_POINT ( 'NONE',  ( 1.567709126316360058, -3.915917399657849796, 2.944712621036570166 ) ) ;
#2575 = CARTESIAN_POINT ( 'NONE',  ( -0.009227126607030738600, -5.296242143452180251, 2.310024366372019688 ) ) ;
#2576 = DIRECTION ( 'NONE',  ( -1.224646799147350002E-16, 1.000000000000000000, 6.123233995736769734E-17 ) ) ;
#2577 = CARTESIAN_POINT ( 'NONE',  ( -2.354888465609351389, -5.502118644067805597, 5.923664702843871588 ) ) ;
#2578 = ORIENTED_EDGE ( 'NONE', *, *, #12979, .T. ) ;
#2579 = VECTOR ( 'NONE', #1024, 1000.000000000000000 ) ;
#2580 = DIRECTION ( 'NONE',  ( 1.000000000000000000, 0.000000000000000000, 0.000000000000000000 ) ) ;
#2581 = AXIS2_PLACEMENT_3D ( 'NONE', #17030, #4355, #8357 ) ;
#2582 = CARTESIAN_POINT ( 'NONE',  ( -1.378221871957429512, -5.179872881355929159, 6.607619368096277590 ) ) ;
#2583 = DIRECTION ( 'NONE',  ( 1.224646799147350002E-16, -1.000000000000000000, -6.123233995736779594E-17 ) ) ;
#2584 = CARTESIAN_POINT ( 'NONE',  ( 0.009452071482872208621, -0.3001926707426449403, 2.353323636140386199 ) ) ;
#2585 = AXIS2_PLACEMENT_3D ( 'NONE', #5428, #11065, #16709 ) ;
#2586 = ORIENTED_EDGE ( 'NONE', *, *, #15498, .T. ) ;
#2587 = AXIS2_PLACEMENT_3D ( 'NONE', #13605, #8055, #919 ) ;
#2588 = VECTOR ( 'NONE', #6221, 1000.000000000000000 ) ;
#2589 = CARTESIAN_POINT ( 'NONE',  ( 2.353452300571019506, -4.125511994252439862, 4.697179287168359529 ) ) ;
#2590 = EDGE_CURVE ( 'NONE', #16690, #7957, #6557, .T. ) ;
#2591 =( LENGTH_UNIT ( ) NAMED_UNIT ( * ) SI_UNIT ( .MILLI., .METRE. ) );
#2592 = CARTESIAN_POINT ( 'NONE',  ( 0.009452110982655383825, -5.000192044704546035, 2.050000000000001155 ) ) ;
#2593 = CARTESIAN_POINT ( 'NONE',  ( -1.250000000000000000, 3.881370849898470254, 6.100000000000000533 ) ) ;
#2594 = EDGE_CURVE ( 'NONE', #4272, #3830, #226, .T. ) ;
#2595 = DIRECTION ( 'NONE',  ( 0.000000000000000000, 1.000000000000000000, 0.000000000000000000 ) ) ;
#2596 = AXIS2_PLACEMENT_3D ( 'NONE', #8427, #9907, #12693 ) ;
#2597 = CARTESIAN_POINT ( 'NONE',  ( -0.7435598031058080482, -3.030962444702889780, 6.932904947974540377 ) ) ;
#2598 = AXIS2_PLACEMENT_3D ( 'NONE', #9789, #13865, #1182 ) ;
#2599 = ADVANCED_FACE ( 'NONE', ( #7762 ), #3587, .F. ) ;
#2600 = CARTESIAN_POINT ( 'NONE',  ( -1.600000000000000089, -9.269168731236219867E-17, 4.000000000000000000 ) ) ;
#2601 = VECTOR ( 'NONE', #10358, 1000.000000000000000 ) ;
#2602 = CARTESIAN_POINT ( 'NONE',  ( -1.992092870331710452, -3.403575057315514130, 4.203544726484199856 ) ) ;
#2603 = CARTESIAN_POINT ( 'NONE',  ( -0.06264882350515391107, -0.4512711864406790396, 7.052569299041220319 ) ) ;
#2604 = DIRECTION ( 'NONE',  ( 1.000000000000000000, -2.220446049250309876E-16, -6.123233995736759873E-17 ) ) ;
#2605 = AXIS2_PLACEMENT_3D ( 'NONE', #17369, #4587, #10160 ) ;
#2606 = CARTESIAN_POINT ( 'NONE',  ( -0.1698804968610999888, -0.2965485159365569556, 2.349238660949160007 ) ) ;
#2607 = ORIENTED_EDGE ( 'NONE', *, *, #14345, .F. ) ;
#2608 = AXIS2_PLACEMENT_3D ( 'NONE', #6376, #9161, #468 ) ;
#2609 = CARTESIAN_POINT ( 'NONE',  ( -1.460675875430050175, -4.684430913171359734, 6.545310725710059785 ) ) ;
#2610 = ORIENTED_EDGE ( 'NONE', *, *, #2590, .F. ) ;
#2611 = VERTEX_POINT ( 'NONE', #16460 ) ;
#2612 = VECTOR ( 'NONE', #15081, 1000.000000000000000 ) ;
#2613 = ORIENTED_EDGE ( 'NONE', *, *, #12876, .T. ) ;
#2614 = PLANE ( 'NONE',  #17676 ) ;
#2615 = CARTESIAN_POINT ( 'NONE',  ( -1.042222075699109407, -5.175423728813555613, 6.468743694056166227 ) ) ;
#2616 = DIRECTION ( 'NONE',  ( -6.123233995736769734E-17, -8.820551857043939970E-15, -1.000000000000000000 ) ) ;
#2617 = CARTESIAN_POINT ( 'NONE',  ( 2.500000000000000000, 0.4000000000000000222, 4.000000000000000000 ) ) ;
#2618 = CARTESIAN_POINT ( 'NONE',  ( -0.1749999999999999889, 7.700000000000000178, 0.5999999999999999778 ) ) ;
#2619 = VECTOR ( 'NONE', #2883, 1000.000000000000000 ) ;
#2620 = CARTESIAN_POINT ( 'NONE',  ( -1.505092429369619955, -5.128627060139309357, 2.879659483602799774 ) ) ;
#2621 = VECTOR ( 'NONE', #11865, 1000.000000000000000 ) ;
#2622 = EDGE_CURVE ( 'NONE', #4099, #13297, #5073, .T. ) ;
#2623 = DIRECTION ( 'NONE',  ( -1.448116988641510032E-16, 0.000000000000000000, -1.000000000000000000 ) ) ;
#2624 = CARTESIAN_POINT ( 'NONE',  ( -2.255259958075430227, -1.703530012270459970, 5.372717034856060003 ) ) ;
#2625 = CARTESIAN_POINT ( 'NONE',  ( -1.932035991685910004, -0.2610169491525428653, 2.884370051397200818 ) ) ;
#2626 = LINE ( 'NONE', #12612, #812 ) ;
#2627 = VERTEX_POINT ( 'NONE', #14800 ) ;
#2628 = CARTESIAN_POINT ( 'NONE',  ( 1.851073041990159984, -0.1067796610169499949, 6.153284478378259870 ) ) ;
#2629 = DIRECTION ( 'NONE',  ( 3.416070845000479880E-16, 1.000000000000000000, 8.540177112501199701E-17 ) ) ;
#2630 = VERTEX_POINT ( 'NONE', #17641 ) ;
#2631 = VECTOR ( 'NONE', #4875, 1000.000000000000000 ) ;
#2632 = AXIS2_PLACEMENT_3D ( 'NONE', #7628, #13275, #10482 ) ;
#2633 = CARTESIAN_POINT ( 'NONE',  ( -1.000000000000000000, -5.599999999999999645, 5.100000000000000533 ) ) ;
#2634 = EDGE_CURVE ( 'NONE', #10238, #11655, #12124, .T. ) ;
#2635 = CARTESIAN_POINT ( 'NONE',  ( -1.724579595320039793, -1.660794312053859745, 3.098572228637930248 ) ) ;
#2636 = CARTESIAN_POINT ( 'NONE',  ( 1.873832970144350130, -5.337500000000000355, 2.826167029855650270 ) ) ;
#2637 = ORIENTED_EDGE ( 'NONE', *, *, #5115, .T. ) ;
#2638 = VECTOR ( 'NONE', #2679, 1000.000000000000000 ) ;
#2639 = CARTESIAN_POINT ( 'NONE',  ( 1.115198193348289957, -1.261052534792989954, 6.772457159276550342 ) ) ;
#2640 = CARTESIAN_POINT ( 'NONE',  ( 2.182690844914370043, -3.919758276017820453, 5.580117243900430068 ) ) ;
#2641 = ORIENTED_EDGE ( 'NONE', *, *, #2055, .F. ) ;
#2642 = EDGE_CURVE ( 'NONE', #1947, #9534, #10247, .T. ) ;
#2643 = CARTESIAN_POINT ( 'NONE',  ( -1.255262969126040791E-16, 7.250000000000000000, 5.100000000000000533 ) ) ;
#2644 = DIRECTION ( 'NONE',  ( 0.000000000000000000, 3.581736239852560511E-31, -1.000000000000000000 ) ) ;
#2645 = AXIS2_PLACEMENT_3D ( 'NONE', #5227, #11989, #16247 ) ;
#2646 = CARTESIAN_POINT ( 'NONE',  ( -2.032257487115171291, -4.571830348089889640, 4.991258216523934976 ) ) ;
#2647 = CARTESIAN_POINT ( 'NONE',  ( 0.6500000000000000222, 6.450000000000000178, 3.200000000000000178 ) ) ;
#2648 = EDGE_LOOP ( 'NONE', ( #15532, #11027, #15752, #1547, #13535, #7723, #5120, #8060, #15565, #11358, #12001, #12405 ) ) ;
#2649 = CARTESIAN_POINT ( 'NONE',  ( 0.000000000000000000, 4.930380657631319405E-32, 8.300000000000000711 ) ) ;
#2650 = DIRECTION ( 'NONE',  ( -1.000000000000000000, 4.956352788505162676E-15, 0.000000000000000000 ) ) ;
#2651 = CARTESIAN_POINT ( 'NONE',  ( -1.494593880360799432, -0.2610169491525428653, 3.295456077495951153 ) ) ;
#2652 = CARTESIAN_POINT ( 'NONE',  ( -1.213493134184840727, -3.314262780522333696, 2.339799138571439396 ) ) ;
#2653 = CARTESIAN_POINT ( 'NONE',  ( -1.458615186838411626, -5.103620102360555855, 3.259477383973569786 ) ) ;
#2654 = CARTESIAN_POINT ( 'NONE',  ( -1.846259792136611066, -5.246610169491530584, 3.802221692020929744 ) ) ;
#2655 = ORIENTED_EDGE ( 'NONE', *, *, #14959, .T. ) ;
#2656 = PLANE ( 'NONE',  #4452 ) ;
#2657 = CARTESIAN_POINT ( 'NONE',  ( 2.058670345754650022, -5.350847457627120107, 3.559656372813920111 ) ) ;
#2658 = VECTOR ( 'NONE', #7781, 1000.000000000000000 ) ;
#2659 = ORIENTED_EDGE ( 'NONE', *, *, #1729, .F. ) ;
#2660 = CARTESIAN_POINT ( 'NONE',  ( -1.057242234132100167, -5.577754237288139905, 2.597442975781530272 ) ) ;
#2661 = CARTESIAN_POINT ( 'NONE',  ( 1.930452136971109622, -4.012911429170968880, 6.521117305355573102 ) ) ;
#2662 = CARTESIAN_POINT ( 'NONE',  ( -1.875000000000000000, 0.7500000000000000000, 7.700000000000000178 ) ) ;
#2663 = CARTESIAN_POINT ( 'NONE',  ( 0.4114611322411816374, -1.032010528270079330, 6.711368086473216366 ) ) ;
#2664 = CARTESIAN_POINT ( 'NONE',  ( 0.2335786437626899970, 3.050000000000000266, 1.958578643762689753 ) ) ;
#2665 = ORIENTED_EDGE ( 'NONE', *, *, #4156, .T. ) ;
#2666 = VECTOR ( 'NONE', #11388, 1000.000000000000000 ) ;
#2667 = ADVANCED_FACE ( 'NONE', ( #10522 ), #7020, .T. ) ;
#2668 = CARTESIAN_POINT ( 'NONE',  ( 1.399999999999999911, 6.400000000000000355, 8.300000000000000711 ) ) ;
#2669 = CARTESIAN_POINT ( 'NONE',  ( -2.332582362116870200, -0.5313559322033900578, 4.387643303570819775 ) ) ;
#2670 = CARTESIAN_POINT ( 'NONE',  ( -2.351526912647309953, -0.5269067796610169552, 4.606040641882809261 ) ) ;
#2671 = CARTESIAN_POINT ( 'NONE',  ( 0.7678268402137939930, -2.867944426684879922, 6.924676972266129660 ) ) ;
#2672 = CARTESIAN_POINT ( 'NONE',  ( -0.5500000000000000444, -2.399999999999999911, 3.299999999999999822 ) ) ;
#2673 = CARTESIAN_POINT ( 'NONE',  ( 2.241103642439659443E-15, 9.099999999999999645, 8.300000000000000711 ) ) ;
#2674 = CARTESIAN_POINT ( 'NONE',  ( 1.873832970144350130, -5.037500000000000533, 2.826167029855650270 ) ) ;
#2675 = ORIENTED_EDGE ( 'NONE', *, *, #4647, .F. ) ;
#2676 = PRESENTATION_STYLE_ASSIGNMENT (( #8145 ) ) ;
#2677 = ORIENTED_EDGE ( 'NONE', *, *, #10536, .T. ) ;
#2678 = CARTESIAN_POINT ( 'NONE',  ( -0.6493550500446438889, -5.286652542372878294, 2.437955526623101665 ) ) ;
#2679 = DIRECTION ( 'NONE',  ( 2.220446049250309876E-16, 4.440892098500630106E-16, -1.000000000000000000 ) ) ;
#2680 = DIRECTION ( 'NONE',  ( 1.445602896647339508E-15, -1.000000000000000000, -1.264902534566422168E-15 ) ) ;
#2681 = VERTEX_POINT ( 'NONE', #4737 ) ;
#2682 = EDGE_CURVE ( 'NONE', #10396, #5167, #4547, .T. ) ;
#2683 = VECTOR ( 'NONE', #242, 1000.000000000000000 ) ;
#2684 = CARTESIAN_POINT ( 'NONE',  ( 1.315859850362970151, -5.328211948015590060, 2.737664967889629875 ) ) ;
#2685 = LINE ( 'NONE', #4155, #13082 ) ;
#2686 = CARTESIAN_POINT ( 'NONE',  ( 4.898587196589409994E-17, 0.1000000000000000056, 8.300000000000000711 ) ) ;
#2687 = CARTESIAN_POINT ( 'NONE',  ( 1.219286470748990103, -4.381683165423610582, 6.712979431025659416 ) ) ;
#2688 = FACE_OUTER_BOUND ( 'NONE', #3433, .T. ) ;
#2689 = CARTESIAN_POINT ( 'NONE',  ( -2.002297259025881182, -3.287133615874059611, 5.153549919110945510 ) ) ;
#2690 = LINE ( 'NONE', #9727, #9050 ) ;
#2691 = AXIS2_PLACEMENT_3D ( 'NONE', #7535, #17431, #4750 ) ;
#2692 = VERTEX_POINT ( 'NONE', #11598 ) ;
#2693 = LINE ( 'NONE', #17021, #2666 ) ;
#2694 = VERTEX_POINT ( 'NONE', #16048 ) ;
#2695 = EDGE_CURVE ( 'NONE', #1663, #2916, #10468, .T. ) ;
#2696 = CARTESIAN_POINT ( 'NONE',  ( 1.850000000000000089, -5.599999999999999645, 6.400000000000000355 ) ) ;
#2697 = CARTESIAN_POINT ( 'NONE',  ( -2.296954468777729463, -4.963890372630819670, 4.187412587068699565 ) ) ;
#2698 = ORIENTED_EDGE ( 'NONE', *, *, #252, .F. ) ;
#2699 = ORIENTED_EDGE ( 'NONE', *, *, #5174, .F. ) ;
#2700 = EDGE_CURVE ( 'NONE', #9144, #7297, #5833, .T. ) ;
#2701 = UNCERTAINTY_MEASURE_WITH_UNIT (LENGTH_MEASURE( 1.000000000000000082E-05 ), #6020, 'distance_accuracy_value', 'NONE');
#2702 = EDGE_CURVE ( 'NONE', #17179, #8282, #7612, .T. ) ;
#2703 = EDGE_LOOP ( 'NONE', ( #8993, #13075, #15401, #10126 ) ) ;
#2704 = LINE ( 'NONE', #12427, #12086 ) ;
#2705 = EDGE_CURVE ( 'NONE', #1300, #2568, #7707, .T. ) ;
#2706 = CARTESIAN_POINT ( 'NONE',  ( 1.994315313497110997, -5.086440677966105994, 5.187224322759965922 ) ) ;
#2707 = ADVANCED_FACE ( 'NONE', ( #6498 ), #15128, .T. ) ;
#2708 = PRODUCT_DEFINITION_SHAPE ( 'NONE', 'NONE',  #18296 ) ;
#2709 = CARTESIAN_POINT ( 'NONE',  ( 2.161103922260819044, -2.103271789531340641, 3.159628768708413915 ) ) ;
#2710 = LINE ( 'NONE', #8269, #3457 ) ;
#2711 = LINE ( 'NONE', #7159, #12638 ) ;
#2712 = ADVANCED_FACE ( 'NONE', ( #11033 ), #6388, .T. ) ;
#2713 = DIRECTION ( 'NONE',  ( 2.220446049250309876E-16, 0.000000000000000000, -1.000000000000000000 ) ) ;
#2714 = LINE ( 'NONE', #28, #1370 ) ;
#2715 = LINE ( 'NONE', #1599, #3175 ) ;
#2716 = CARTESIAN_POINT ( 'NONE',  ( 1.115198193348289957, -1.261052534792989954, 6.772457159276550342 ) ) ;
#2717 = CARTESIAN_POINT ( 'NONE',  ( -2.007801995112629356, -2.988226744486289999, 5.128524201241715375 ) ) ;
#2718 = CARTESIAN_POINT ( 'NONE',  ( -1.641808337277740115, -0.1868644067796620123, 6.386111670537629514 ) ) ;
#2719 = EDGE_CURVE ( 'NONE', #14928, #14013, #7995, .T. ) ;
#2720 = VERTEX_POINT ( 'NONE', #3989 ) ;
#2721 = CARTESIAN_POINT ( 'NONE',  ( -2.328217775191430139, -0.5180084745762719711, 5.043379051721170292 ) ) ;
#2722 = PLANE ( 'NONE',  #3827 ) ;
#2723 = EDGE_LOOP ( 'NONE', ( #1474, #10302, #4304, #11286 ) ) ;
#2724 = CARTESIAN_POINT ( 'NONE',  ( -0.06264882350515391107, -0.1512711864406779960, 7.052569299041220319 ) ) ;
#2725 = CARTESIAN_POINT ( 'NONE',  ( 0.9170541073686970801, -1.284340823081270067, 6.867431071947180499 ) ) ;
#2726 = ORIENTED_EDGE ( 'NONE', *, *, #11703, .F. ) ;
#2727 = CARTESIAN_POINT ( 'NONE',  ( 3.371799150351489833E-16, 2.299999999999999822, 7.700000000000000178 ) ) ;
#2728 = EDGE_CURVE ( 'NONE', #8832, #8965, #17864, .T. ) ;
#2729 = ORIENTED_EDGE ( 'NONE', *, *, #3034, .F. ) ;
#2730 = CARTESIAN_POINT ( 'NONE',  ( 2.295719155670170153, -2.312866384125930264, 5.218091927917189565 ) ) ;
#2731 =( NAMED_UNIT ( * ) SI_UNIT ( $, .STERADIAN. ) SOLID_ANGLE_UNIT ( ) );
#2732 = CARTESIAN_POINT ( 'NONE',  ( 1.031876288691629506, -5.430932203389830626, 7.145012538880298081 ) ) ;
#2733 = ORIENTED_EDGE ( 'NONE', *, *, #10055, .T. ) ;
#2734 = DIRECTION ( 'NONE',  ( -1.000000000000000000, 6.161988852941170860E-64, 6.123233995736769734E-17 ) ) ;
#2735 = CARTESIAN_POINT ( 'NONE',  ( 1.248294325655350034, -0.3266949152542379942, 2.704938983774300088 ) ) ;
#2736 = EDGE_LOOP ( 'NONE', ( #9267, #10945, #16466 ) ) ;
#2737 = CARTESIAN_POINT ( 'NONE',  ( 0.1749999999999999889, 9.299999999999998934, 1.600000000000000089 ) ) ;
#2738 = LINE ( 'NONE', #8566, #7038 ) ;
#2739 = DIRECTION ( 'NONE',  ( 1.000000000000000000, -8.673617379884035472E-15, 0.000000000000000000 ) ) ;
#2740 = CARTESIAN_POINT ( 'NONE',  ( 1.872456193198871022, -1.098034516774970770, 5.541908336565965598 ) ) ;
#2741 = DIRECTION ( 'NONE',  ( 1.224646799147350002E-16, -1.000000000000000000, -6.123233995736769734E-17 ) ) ;
#2742 = VERTEX_POINT ( 'NONE', #17958 ) ;
#2743 = PLANE ( 'NONE',  #88 ) ;
#2744 = DIRECTION ( 'NONE',  ( 0.000000000000000000, 0.000000000000000000, 1.000000000000000000 ) ) ;
#2745 = AXIS2_PLACEMENT_3D ( 'NONE', #8071, #13711, #9339 ) ;
#2746 = EDGE_CURVE ( 'NONE', #12789, #3214, #17775, .T. ) ;
#2747 = CARTESIAN_POINT ( 'NONE',  ( -0.9880847989278745969, -3.337551068810613142, 2.236912075639700515 ) ) ;
#2748 = CARTESIAN_POINT ( 'NONE',  ( 0.3367924244280819934, 2.254758922476410188, 8.300000000000000711 ) ) ;
#2749 = CARTESIAN_POINT ( 'NONE',  ( 0.4339619423229844619, -5.139830508474575232, 6.706578715862737461 ) ) ;
#2750 = EDGE_LOOP ( 'NONE', ( #16890, #17506, #9063, #3086 ) ) ;
#2751 = EDGE_CURVE ( 'NONE', #16690, #3782, #5109, .T. ) ;
#2752 = AXIS2_PLACEMENT_3D ( 'NONE', #6090, #16341, #3318 ) ;
#2753 = CARTESIAN_POINT ( 'NONE',  ( 2.253200202764419569, -0.08898305084745812554, 5.379408587037500133 ) ) ;
#2754 = CARTESIAN_POINT ( 'NONE',  ( -1.399999999999999911, 6.400000000000000355, 7.700000000000000178 ) ) ;
#2755 = CARTESIAN_POINT ( 'NONE',  ( -0.9290506585603975909, -0.5829339996946386604, 2.210445150547709403 ) ) ;
#2756 = EDGE_LOOP ( 'NONE', ( #16576, #2138, #5022, #5992 ) ) ;
#2757 = SHAPE_REPRESENTATION ( 'MAS-687', ( #11212, #4400, #15364, #14162, #14739, #5885, #3505, #16224, #1751, #8257, #9731, #10599 ), #861 ) ;
#2758 = DIRECTION ( 'NONE',  ( 0.000000000000000000, -1.000000000000000000, 0.000000000000000000 ) ) ;
#2759 = CARTESIAN_POINT ( 'NONE',  ( 2.135041058613650122, -0.7991276453871950514, 5.690123914223769397 ) ) ;
#2760 = CARTESIAN_POINT ( 'NONE',  ( -2.350000000000000089, -6.000000000000000000, 6.400000000000000355 ) ) ;
#2761 = DIRECTION ( 'NONE',  ( -1.110223024625159992E-16, 0.000000000000000000, 1.000000000000000000 ) ) ;
#2762 = VERTEX_POINT ( 'NONE', #15309 ) ;
#2763 = CARTESIAN_POINT ( 'NONE',  ( 1.290000000000029790, 4.099999999999997868, 3.000000000000006661 ) ) ;
#2764 = CARTESIAN_POINT ( 'NONE',  ( 2.306642602145299925, -0.3845338983050849979, 5.166805192608480368 ) ) ;
#2765 = CARTESIAN_POINT ( 'NONE',  ( -0.6918414964982418924, -3.659746228486680408, 2.450533167346770291 ) ) ;
#2766 = CARTESIAN_POINT ( 'NONE',  ( -1.000000000000000000, -5.500000000000000000, 5.100000000000000533 ) ) ;
#2767 = LINE ( 'NONE', #7130, #16859 ) ;
#2768 = CARTESIAN_POINT ( 'NONE',  ( 2.625437065641401446, -5.081991525423726230, 5.087214675345139270 ) ) ;
#2769 = ORIENTED_EDGE ( 'NONE', *, *, #3915, .T. ) ;
#2770 = ORIENTED_EDGE ( 'NONE', *, *, #3686, .F. ) ;
#2771 = CARTESIAN_POINT ( 'NONE',  ( -2.203023580854000851, -5.242161016949149044, 3.872235369154300333 ) ) ;
#2772 = CARTESIAN_POINT ( 'NONE',  ( 0.7500000000000000000, 6.450000000000000178, 2.699264068711930253 ) ) ;
#2773 = ORIENTED_EDGE ( 'NONE', *, *, #659, .T. ) ;
#2774 = AXIS2_PLACEMENT_3D ( 'NONE', #7737, #6071, #1829 ) ;
#2775 = CARTESIAN_POINT ( 'NONE',  ( 1.032615103526660416, -1.284340823081270733, 7.144753513336372208 ) ) ;
#2776 = CARTESIAN_POINT ( 'NONE',  ( 0.2554393686801398333, -0.6247245358507580448, 2.048880876762550596 ) ) ;
#2777 = CARTESIAN_POINT ( 'NONE',  ( 1.484081582636959551, -5.328211948015596278, 2.487334927317659705 ) ) ;
#2778 = LINE ( 'NONE', #9717, #151 ) ;
#2779 = CARTESIAN_POINT ( 'NONE',  ( 0.9000000000000000222, -9.500000000000000000, 6.100000000000000533 ) ) ;
#2780 = CARTESIAN_POINT ( 'NONE',  ( -1.286937324407759986, -3.589881363621809651, 2.729584305145209999 ) ) ;
#2781 = VECTOR ( 'NONE', #7671, 1000.000000000000000 ) ;
#2782 = CARTESIAN_POINT ( 'NONE',  ( -2.500000000000000000, 2.799999999999999822, 1.600000000000000089 ) ) ;
#2783 = CARTESIAN_POINT ( 'NONE',  ( -1.313542260532420292, -3.124115597856051085, 6.277817661335885369 ) ) ;
#2784 = DIRECTION ( 'NONE',  ( 0.000000000000000000, 0.000000000000000000, 1.000000000000000000 ) ) ;
#2785 = VERTEX_POINT ( 'NONE', #6679 ) ;
#2786 = CARTESIAN_POINT ( 'NONE',  ( -0.1869574461324000070, -0.5962015548080630278, 2.350675676344399889 ) ) ;
#2787 = VERTEX_POINT ( 'NONE', #16317 ) ;
#2788 = CYLINDRICAL_SURFACE ( 'NONE', #9885, 0.4999999999999995559 ) ;
#2789 = ORIENTED_EDGE ( 'NONE', *, *, #8245, .F. ) ;
#2790 = ORIENTED_EDGE ( 'NONE', *, *, #2363, .F. ) ;
#2791 = CARTESIAN_POINT ( 'NONE',  ( -2.500000000000000000, 2.799999999999999822, 1.600000000000000089 ) ) ;
#2792 = EDGE_LOOP ( 'NONE', ( #11954, #5924, #2083, #11587 ) ) ;
#2793 = DIRECTION ( 'NONE',  ( -2.018587317500279868E-16, 1.000000000000000000, 1.009293658750139934E-16 ) ) ;
#2794 = CARTESIAN_POINT ( 'NONE',  ( -0.6493550500446439999, -5.286652542372879182, 2.437955526623099889 ) ) ;
#2795 = CARTESIAN_POINT ( 'NONE',  ( -2.247144151254851341, -1.614217735477279536, 3.288101683376949413 ) ) ;
#2796 = DIRECTION ( 'NONE',  ( -6.740754805355319355E-31, 1.000000000000000000, -1.040834085586083310E-14 ) ) ;
#2797 = CARTESIAN_POINT ( 'NONE',  ( 1.708406120534559980, -0.7760574766851200401, 2.975829173059839849 ) ) ;
#2798 = CARTESIAN_POINT ( 'NONE',  ( 2.500000000000000000, 2.000000000000000000, -1.695950706916410117E-15 ) ) ;
#2799 = DIRECTION ( 'NONE',  ( 0.000000000000000000, 0.000000000000000000, -1.000000000000000000 ) ) ;
#2800 = CARTESIAN_POINT ( 'NONE',  ( -1.250000000000000000, 0.5999999999999999778, 7.599999999999999645 ) ) ;
#2801 = CARTESIAN_POINT ( 'NONE',  ( 2.126557263589630153, -2.448755237495689574, 3.691783806836010040 ) ) ;
#2802 = CARTESIAN_POINT ( 'NONE',  ( -1.538437905835030595, -3.221109627369172390, 3.340547664492051094 ) ) ;
#2803 = EDGE_CURVE ( 'NONE', #8504, #2212, #1393, .T. ) ;
#2804 = CARTESIAN_POINT ( 'NONE',  ( -2.332582362116870200, -0.2313559322033900134, 4.387643303570819775 ) ) ;
#2805 = VERTEX_POINT ( 'NONE', #3815 ) ;
#2806 = CARTESIAN_POINT ( 'NONE',  ( -0.4974685680287780354, -0.4601694915254240237, 7.000224381598740386 ) ) ;
#2807 = ADVANCED_FACE ( 'NONE', ( #13444 ), #5305, .T. ) ;
#2808 = ADVANCED_FACE ( 'NONE', ( #10672 ), #3621, .F. ) ;
#2809 = CARTESIAN_POINT ( 'NONE',  ( 1.899999999999999911, 0.7211102550927980248, 4.000000000000000000 ) ) ;
#2810 = ORIENTED_EDGE ( 'NONE', *, *, #7560, .F. ) ;
#2811 = CARTESIAN_POINT ( 'NONE',  ( -1.791574935211209807, -0.1913135593220340047, 6.226029630577610163 ) ) ;
#2812 = CARTESIAN_POINT ( 'NONE',  ( -0.8001898266890440370, -1.470647129387580021, 6.913242401714570384 ) ) ;
#2813 = ORIENTED_EDGE ( 'NONE', *, *, #3828, .F. ) ;
#2814 = CARTESIAN_POINT ( 'NONE',  ( 0.5000000000000000000, 4.631370849898480024, 5.100000000000000533 ) ) ;
#2815 = ORIENTED_EDGE ( 'NONE', *, *, #14060, .F. ) ;
#2816 = CARTESIAN_POINT ( 'NONE',  ( 1.630481553867769495, -2.056695212954760432, 3.002862530617849579 ) ) ;
#2817 = CARTESIAN_POINT ( 'NONE',  ( -2.011500846714319835, -5.551059322033900401, 3.478373409938470218 ) ) ;
#2818 = ORIENTED_EDGE ( 'NONE', *, *, #8134, .T. ) ;
#2819 = CARTESIAN_POINT ( 'NONE',  ( 1.850000000000000089, -5.599999999999999645, 6.899999999999999467 ) ) ;
#2820 = CARTESIAN_POINT ( 'NONE',  ( -1.940327948426050941, -0.5091101694915260989, 5.370677689277675526 ) ) ;
#2821 = ORIENTED_EDGE ( 'NONE', *, *, #662, .T. ) ;
#2822 = ADVANCED_FACE ( 'NONE', ( #15031 ), #3181, .T. ) ;
#2823 = DIRECTION ( 'NONE',  ( 0.000000000000000000, -1.000000000000000000, 0.000000000000000000 ) ) ;
#2824 = CARTESIAN_POINT ( 'NONE',  ( -2.350000000000000089, -5.599999999999999645, 6.400000000000000355 ) ) ;
#2825 = CARTESIAN_POINT ( 'NONE',  ( 0.3943683997329633373, -2.215872354612800521, 2.685210827922638543 ) ) ;
#2827 = EDGE_CURVE ( 'NONE', #1696, #1947, #14158, .T. ) ;
#2826 = CARTESIAN_POINT ( 'NONE',  ( 0.1749999999999999889, 8.200000000000001066, 0.4000000000000000222 ) ) ;
#2828 = VERTEX_POINT ( 'NONE', #6391 ) ;
#2829 = DIRECTION ( 'NONE',  ( -1.000000000000000000, 2.891205793294678228E-15, 3.614007241618347587E-15 ) ) ;
#2830 = FACE_OUTER_BOUND ( 'NONE', #17027, .T. ) ;
#2831 = DIRECTION ( 'NONE',  ( -3.042833474898580443E-15, 3.289549702593060178E-16, 1.000000000000000000 ) ) ;
#2832 = CARTESIAN_POINT ( 'NONE',  ( -0.06367493584607197832, -5.598516949152545941, 2.649999999999998579 ) ) ;
#2833 = VERTEX_POINT ( 'NONE', #4649 ) ;
#2834 = CARTESIAN_POINT ( 'NONE',  ( 0.1749999999999999889, 9.500000000000000000, 1.600000000000000089 ) ) ;
#2835 = CARTESIAN_POINT ( 'NONE',  ( -1.661700935788390066, -0.4124999999999999778, 3.038299064211610112 ) ) ;
#2836 = CARTESIAN_POINT ( 'NONE',  ( -0.4617942143426889690, -0.5906145504024210569, 2.383143958488499692 ) ) ;
#2837 = ORIENTED_EDGE ( 'NONE', *, *, #17107, .F. ) ;
#2838 = DIRECTION ( 'NONE',  ( 1.110223024625159992E-16, 0.000000000000000000, -1.000000000000000000 ) ) ;
#2839 = CARTESIAN_POINT ( 'NONE',  ( 1.092567884283869972, -0.9621456634052130141, 6.784476218553570526 ) ) ;
#2840 = CARTESIAN_POINT ( 'NONE',  ( 1.983927814618709085E-15, 11.43245553203367493, 7.700000000000000178 ) ) ;
#2841 = EDGE_CURVE ( 'NONE', #12458, #7208, #6113, .T. ) ;
#2842 = CARTESIAN_POINT ( 'NONE',  ( 0.9516466452860694591, -0.9621456634052125700, 6.519140045500582126 ) ) ;
#2843 = AXIS2_PLACEMENT_3D ( 'NONE', #12501, #13713, #13522 ) ;
#2845 = EDGE_CURVE ( 'NONE', #4577, #12789, #10567, .T. ) ;
#2844 = CARTESIAN_POINT ( 'NONE',  ( 0.5500000000000000444, 6.450000000000000178, 3.299999999999999822 ) ) ;
#2846 = ORIENTED_EDGE ( 'NONE', *, *, #1578, .F. ) ;
#2847 = DIRECTION ( 'NONE',  ( -0.06030856937325100586, -0.9963562379592471041, 0.06030856937324956257 ) ) ;
#2848 = CARTESIAN_POINT ( 'NONE',  ( -1.811729841638700211, -0.5580508474576270084, 3.197954009834299782 ) ) ;
#2849 = CARTESIAN_POINT ( 'NONE',  ( -2.143090896833110381, -0.5046610169491529962, 5.672454929438350391 ) ) ;
#2850 = CARTESIAN_POINT ( 'NONE',  ( -1.816660071039029933, -3.170692174432619748, 6.196159040268240936 ) ) ;
#2851 = CARTESIAN_POINT ( 'NONE',  ( -1.000000000000000000, 6.799999999999999822, 7.700000000000000178 ) ) ;
#2852 = LINE ( 'NONE', #16731, #7401 ) ;
#2853 = CARTESIAN_POINT ( 'NONE',  ( -2.653602652190420574, -5.524364406779660897, 4.735326402787099376 ) ) ;
#2854 = ORIENTED_EDGE ( 'NONE', *, *, #8846, .T. ) ;
#2855 = ORIENTED_EDGE ( 'NONE', *, *, #15995, .F. ) ;
#2856 = DIRECTION ( 'NONE',  ( 2.960594732333750117E-15, 0.000000000000000000, -1.000000000000000000 ) ) ;
#2857 = CARTESIAN_POINT ( 'NONE',  ( 1.000000000000000000, 6.799999999999999822, 8.300000000000000711 ) ) ;
#2858 = CARTESIAN_POINT ( 'NONE',  ( 1.610148362874519901, -0.7839942975846440065, 3.073126113101479984 ) ) ;
#2859 = CLOSED_SHELL ( 'NONE', ( #4991, #6069, #15732, #14932, #10275, #3404, #7342, #3353, #1611, #2822, #6796, #13620, #3188, #6203, #676, #9224, #10470, #17040, #6918, #17168, #3251, #6770, #14239, #10827, #14022, #17123, #17821, #17132, #17434, #6408, #7874, #4040, #15633, #2130, #1883, #7239, #11431, #3663, #10083, #3443, #6111, #4390 ) ) ;
#2860 = VERTEX_POINT ( 'NONE', #16053 ) ;
#2861 = VECTOR ( 'NONE', #3010, 1000.000000000000000 ) ;
#2862 = CARTESIAN_POINT ( 'NONE',  ( 2.650521604678268694, -1.004881363621820567, 4.833599835830299618 ) ) ;
#2863 = FILL_AREA_STYLE ('',( #2966 ) ) ;
#2864 = CARTESIAN_POINT ( 'NONE',  ( 1.730954623551391736, -5.333856471231995577, 2.683219139909288842 ) ) ;
#2865 = LINE ( 'NONE', #14165, #17559 ) ;
#2866 = CARTESIAN_POINT ( 'NONE',  ( 2.033393610350129777, -0.8224159336754830463, 5.884928737465320303 ) ) ;
#2868 = EDGE_CURVE ( 'NONE', #1588, #651, #14841, .T. ) ;
#2867 = FACE_OUTER_BOUND ( 'NONE', #1316, .T. ) ;
#2869 = CARTESIAN_POINT ( 'NONE',  ( -0.04278372834682089842, -3.729611093351540063, 2.346934926511239805 ) ) ;
#2870 = DIRECTION ( 'NONE',  ( -1.480297366166879989E-16, 1.000000000000000000, 1.480297366166879989E-16 ) ) ;
#2871 = VECTOR ( 'NONE', #14711, 1000.000000000000000 ) ;
#2872 = CARTESIAN_POINT ( 'NONE',  ( 0.8493734496528324573, -2.844656138396588929, 6.569081749323157915 ) ) ;
#2873 = VECTOR ( 'NONE', #1842, 1000.000000000000000 ) ;
#2874 = FACE_OUTER_BOUND ( 'NONE', #13634, .T. ) ;
#2875 = AXIS2_PLACEMENT_3D ( 'NONE', #9779, #15529, #16633 ) ;
#2876 = ORIENTED_EDGE ( 'NONE', *, *, #16604, .F. ) ;
#2877 = LINE ( 'NONE', #5468, #7668 ) ;
#2878 = VERTEX_POINT ( 'NONE', #12062 ) ;
#2879 = DIRECTION ( 'NONE',  ( 0.000000000000000000, 0.000000000000000000, 1.000000000000000000 ) ) ;
#2880 = ORIENTED_EDGE ( 'NONE', *, *, #17162, .F. ) ;
#2881 = DIRECTION ( 'NONE',  ( 1.000000000000000000, 0.000000000000000000, 0.000000000000000000 ) ) ;
#2882 = AXIS2_PLACEMENT_3D ( 'NONE', #10471, #7525, #9646 ) ;
#2883 = DIRECTION ( 'NONE',  ( -1.000000000000000000, 0.000000000000000000, 0.000000000000000000 ) ) ;
#2884 = VECTOR ( 'NONE', #17075, 1000.000000000000000 ) ;
#2885 = ORIENTED_EDGE ( 'NONE', *, *, #8331, .F. ) ;
#2886 = CARTESIAN_POINT ( 'NONE',  ( -1.965557623688110933, -5.211016949152535993, 5.292675575926340414 ) ) ;
#2887 = CARTESIAN_POINT ( 'NONE',  ( -0.6890111762203582346, -1.800524041783588824, 2.137115435286770282 ) ) ;
#2888 = AXIS2_PLACEMENT_3D ( 'NONE', #1438, #11148, #5503 ) ;
#2889 = CARTESIAN_POINT ( 'NONE',  ( -1.899999999999999911, 3.774758283725530167E-16, 9.441371669411539713 ) ) ;
#2890 = CIRCLE ( 'NONE', #7590, 0.6324555320336745501 ) ;
#2891 = CARTESIAN_POINT ( 'NONE',  ( 1.766949157924760261, -0.6011269801779139943, 2.938462914781730273 ) ) ;
#2892 = ADVANCED_FACE ( 'NONE', ( #14563 ), #11798, .T. ) ;
#2893 = CARTESIAN_POINT ( 'NONE',  ( -2.500000000000000000, 4.700000000000000178, 0.6099999999999999867 ) ) ;
#2894 = DIRECTION ( 'NONE',  ( 0.000000000000000000, 1.332267629550190018E-15, -1.000000000000000000 ) ) ;
#2895 = CARTESIAN_POINT ( 'NONE',  ( 0.5500000000000000444, 6.450000000000000178, 2.699264068711930253 ) ) ;
#2896 = DIRECTION ( 'NONE',  ( 2.220446049250309876E-16, 2.960594732333750117E-16, -1.000000000000000000 ) ) ;
#2897 = CARTESIAN_POINT ( 'NONE',  ( 0.01716182025089369942, -2.169295778036230082, 2.346608583467340026 ) ) ;
#2898 = AXIS2_PLACEMENT_3D ( 'NONE', #2889, #4258, #1594 ) ;
#2899 = CARTESIAN_POINT ( 'NONE',  ( 0.3681613504764975620, -3.477280798540335560, 2.680257674196191431 ) ) ;
#2900 = AXIS2_PLACEMENT_3D ( 'NONE', #8717, #7508, #1515 ) ;
#2901 = CARTESIAN_POINT ( 'NONE',  ( -0.9150601050661559821, -0.1690677966101700180, 6.868218666554230190 ) ) ;
#2902 = CARTESIAN_POINT ( 'NONE',  ( -0.003440977838559869991, -5.204536585018660233, 2.491636233962249758 ) ) ;
#2903 = ADVANCED_FACE ( 'NONE', ( #12162 ), #10765, .F. ) ;
#2904 = LINE ( 'NONE', #8718, #10631 ) ;
#2905 = VERTEX_POINT ( 'NONE', #15313 ) ;
#2906 = AXIS2_PLACEMENT_3D ( 'NONE', #12827, #2744, #12460 ) ;
#2907 = CARTESIAN_POINT ( 'NONE',  ( 2.318251751302029984, -0.06673728813559359763, 4.294764266798990704 ) ) ;
#2908 = CARTESIAN_POINT ( 'NONE',  ( -1.381042549632419902, -1.540511994252449890, 6.605640880016140137 ) ) ;
#2909 = ORIENTED_EDGE ( 'NONE', *, *, #6580, .T. ) ;
#2910 = ORIENTED_EDGE ( 'NONE', *, *, #3519, .T. ) ;
#2911 = CARTESIAN_POINT ( 'NONE',  ( -1.021156010535439584, -1.753947465207010614, 2.579625955254301051 ) ) ;
#2912 = CARTESIAN_POINT ( 'NONE',  ( -2.540842781840720654, -5.511016949152534927, 5.466141598148674952 ) ) ;
#2914 = VECTOR ( 'NONE', #5417, 1000.000000000000000 ) ;
#2913 = MECHANICAL_DESIGN_GEOMETRIC_PRESENTATION_REPRESENTATION (  '', ( #4377 ), #14138 ) ;
#2915 = CIRCLE ( 'NONE', #11775, 0.4000000000000001887 ) ;
#2916 = VERTEX_POINT ( 'NONE', #16603 ) ;
#2917 = CARTESIAN_POINT ( 'NONE',  ( -1.003115764947269950, -1.493935417675869903, 6.828967930617589666 ) ) ;
#2918 = EDGE_CURVE ( 'NONE', #16759, #1710, #5309, .T. ) ;
#2919 = CARTESIAN_POINT ( 'NONE',  ( -1.695509042132779864, -0.5536016949152540167, 3.542446458728619518 ) ) ;
#2920 = ORIENTED_EDGE ( 'NONE', *, *, #5177, .T. ) ;
#2921 = VECTOR ( 'NONE', #7699, 1000.000000000000000 ) ;
#2922 = DIRECTION ( 'NONE',  ( -1.644774851296529842E-16, 1.000000000000000000, 0.000000000000000000 ) ) ;
#2923 = CARTESIAN_POINT ( 'NONE',  ( 2.616666666666660035, -5.805074450128190455E-17, 4.000000000000000000 ) ) ;
#2924 = CARTESIAN_POINT ( 'NONE',  ( 1.019987577504959608, -2.821367850108300157, 6.481720287913791623 ) ) ;
#2925 = DIRECTION ( 'NONE',  ( -1.000000000000000000, 0.000000000000000000, 0.000000000000000000 ) ) ;
#2926 = CARTESIAN_POINT ( 'NONE',  ( 0.7322514394120266390, -0.3133474576271193524, 2.149183891723918993 ) ) ;
#2927 = ORIENTED_EDGE ( 'NONE', *, *, #8577, .F. ) ;
#2928 = CARTESIAN_POINT ( 'NONE',  ( -1.505092429369619955, -5.128627060139309357, 2.879659483602799774 ) ) ;
#2929 = CARTESIAN_POINT ( 'NONE',  ( -1.899999999999999911, 10.00000000000000000, 1.600000000000000089 ) ) ;
#2930 = VECTOR ( 'NONE', #15674, 1000.000000000000000 ) ;
#2931 = ORIENTED_EDGE ( 'NONE', *, *, #15210, .T. ) ;
#2932 = CARTESIAN_POINT ( 'NONE',  ( -1.670747221194380128, -5.103620102360550526, 3.047345349617600174 ) ) ;
#2933 = CARTESIAN_POINT ( 'NONE',  ( -2.052786957354850728, -5.524364406779660897, 4.727327971967373976 ) ) ;
#2934 = VECTOR ( 'NONE', #2961, 1000.000000000000000 ) ;
#2935 = EDGE_CURVE ( 'NONE', #14122, #917, #955, .T. ) ;
#2936 = CARTESIAN_POINT ( 'NONE',  ( 1.057242234132089731, -0.02224576271186470139, 2.597442975781520946 ) ) ;
#2937 = CARTESIAN_POINT ( 'NONE',  ( 0.4974685680287860290, -5.439830508474580384, 7.000224381598740386 ) ) ;
#2938 = DIRECTION ( 'NONE',  ( 0.000000000000000000, 0.000000000000000000, 1.000000000000000000 ) ) ;
#2939 = EDGE_CURVE ( 'NONE', #9877, #17390, #15131, .T. ) ;
#2940 = EDGE_CURVE ( 'NONE', #16382, #12528, #16319, .T. ) ;
#2941 = ORIENTED_EDGE ( 'NONE', *, *, #13967, .T. ) ;
#2942 = CIRCLE ( 'NONE', #12107, 0.2000000000000000389 ) ;
#2943 = CARTESIAN_POINT ( 'NONE',  ( -2.342931736853879787, -1.497776294035840117, 4.477701633099189671 ) ) ;
#2944 = EDGE_CURVE ( 'NONE', #1801, #14551, #5112, .T. ) ;
#2945 = CARTESIAN_POINT ( 'NONE',  ( -1.899999999999999911, 10.00000000000000000, 1.600000000000000089 ) ) ;
#2946 = CARTESIAN_POINT ( 'NONE',  ( 0.9588981328681075444, -1.986830348089900777, 2.884671871696430578 ) ) ;
#2947 = LINE ( 'NONE', #15641, #10254 ) ;
#2948 = VERTEX_POINT ( 'NONE', #5196 ) ;
#2949 = ORIENTED_EDGE ( 'NONE', *, *, #17956, .T. ) ;
#2950 = CARTESIAN_POINT ( 'NONE',  ( 1.689971836761019919, -5.333928624509660210, 3.010028163238979815 ) ) ;
#2951 = CARTESIAN_POINT ( 'NONE',  ( -1.851400890972779045, -0.4868644067796619179, 6.601359968904141340 ) ) ;
#2952 = VECTOR ( 'NONE', #13895, 1000.000000000000000 ) ;
#2953 = CARTESIAN_POINT ( 'NONE',  ( -0.5320716618283710675, -3.007674156414609890, 6.992519451207139802 ) ) ;
#2954 = DIRECTION ( 'NONE',  ( -3.652293603810800245E-15, -1.332267629550183904E-15, 1.000000000000000000 ) ) ;
#2955 = LINE ( 'NONE', #8229, #14494 ) ;
#2956 = CARTESIAN_POINT ( 'NONE',  ( 1.254903241568450900, -5.126483050847465250, 7.038391080368498365 ) ) ;
#2957 = ORIENTED_EDGE ( 'NONE', *, *, #10065, .T. ) ;
#2958 = EDGE_CURVE ( 'NONE', #8588, #2335, #16408, .T. ) ;
#2959 = ORIENTED_EDGE ( 'NONE', *, *, #18057, .T. ) ;
#2960 = DIRECTION ( 'NONE',  ( -0.7071067811865475727, 0.000000000000000000, 0.7071067811865475727 ) ) ;
#2961 = DIRECTION ( 'NONE',  ( -1.000000000000000000, -7.401486830834380223E-16, 6.123233995736769734E-17 ) ) ;
#2962 = LINE ( 'NONE', #10082, #7056 ) ;
#2963 = EDGE_CURVE ( 'NONE', #4577, #9295, #6684, .T. ) ;
#2964 = ORIENTED_EDGE ( 'NONE', *, *, #6783, .F. ) ;
#2965 = CARTESIAN_POINT ( 'NONE',  ( -0.6672256841320821641, -1.447358841099289251, 7.268642361138727637 ) ) ;
#2966 = FILL_AREA_STYLE_COLOUR ( '', #5562 ) ;
#2967 = CARTESIAN_POINT ( 'NONE',  ( 1.449568901432419343, -5.037500000000000533, 3.250431098567584165 ) ) ;
#2968 = VECTOR ( 'NONE', #7672, 1000.000000000000000 ) ;
#2969 = LINE ( 'NONE', #601, #9009 ) ;
#2970 = CARTESIAN_POINT ( 'NONE',  ( 2.351999299633229956, -2.266289807549350055, 4.782734406438239994 ) ) ;
#2971 = DIRECTION ( 'NONE',  ( 1.224646799147349016E-16, 0.000000000000000000, 1.000000000000000000 ) ) ;
#2972 = CARTESIAN_POINT ( 'NONE',  ( 0.1824815401350060040, -4.498124606865050445, 7.046368721022729709 ) ) ;
#2973 = LINE ( 'NONE', #13974, #9031 ) ;
#2974 = CARTESIAN_POINT ( 'NONE',  ( 2.053018524985070314, -4.125511994252439862, 4.695903819313355321 ) ) ;
#2975 = EDGE_CURVE ( 'NONE', #5888, #15231, #1140, .T. ) ;
#2976 = CARTESIAN_POINT ( 'NONE',  ( -9.868649107779171166E-17, -3.700743415417190112E-17, 0.5999999999999999778 ) ) ;
#2977 = ORIENTED_EDGE ( 'NONE', *, *, #2369, .F. ) ;
#2978 = LINE ( 'NONE', #8699, #13290 ) ;
#2979 = EDGE_LOOP ( 'NONE', ( #2180, #17980, #7832, #15856 ) ) ;
#2980 = CARTESIAN_POINT ( 'NONE',  ( 2.500000000000000000, 11.29999999999999893, 7.649999999999999467 ) ) ;
#2981 = ORIENTED_EDGE ( 'NONE', *, *, #6014, .F. ) ;
#2982 = DIRECTION ( 'NONE',  ( -2.055968564120659776E-16, -1.000000000000000000, 0.000000000000000000 ) ) ;
#2983 = EDGE_CURVE ( 'NONE', #15103, #17501, #15015, .T. ) ;
#2984 = ORIENTED_EDGE ( 'NONE', *, *, #8247, .F. ) ;
#2985 = CARTESIAN_POINT ( 'NONE',  ( 1.940327948426050941, -5.390889830508485581, 5.370677689277660427 ) ) ;
#2986 = CARTESIAN_POINT ( 'NONE',  ( -5.045174592681759329E-16, -1.399999999999999911, 5.100000000000000533 ) ) ;
#2987 = DIRECTION ( 'NONE',  ( -1.000000000000000000, 0.000000000000000000, 6.123233995736769734E-17 ) ) ;
#2988 = FACE_OUTER_BOUND ( 'NONE', #6624, .T. ) ;
#2989 = CARTESIAN_POINT ( 'NONE',  ( 6.429395695523600208E-16, 3.500000000000000000, 6.100000000000000533 ) ) ;
#2990 = FACE_OUTER_BOUND ( 'NONE', #11391, .T. ) ;
#2991 = CARTESIAN_POINT ( 'NONE',  ( 0.2335786437626899970, 3.050000000000000266, 2.241421356237310203 ) ) ;
#2992 = AXIS2_PLACEMENT_3D ( 'NONE', #8332, #9707, #1368 ) ;
#2993 = CARTESIAN_POINT ( 'NONE',  ( -0.8429265834919730249, -2.076142624883080323, 2.502678798553459760 ) ) ;
#2994 = CARTESIAN_POINT ( 'NONE',  ( -1.985741519624380835, -3.104668185927728974, 4.178720363079513334 ) ) ;
#2995 = CARTESIAN_POINT ( 'NONE',  ( -2.143090896833110381, -0.2046610169491530073, 5.672454929438350391 ) ) ;
#2996 = CARTESIAN_POINT ( 'NONE',  ( 0.009452071482871029010, -5.000192670742644729, 2.353323636140357333 ) ) ;
#2997 = DIRECTION ( 'NONE',  ( 1.000000000000000000, -2.220446049250309876E-16, 0.000000000000000000 ) ) ;
#2998 = ORIENTED_EDGE ( 'NONE', *, *, #1154, .T. ) ;
#2999 = CARTESIAN_POINT ( 'NONE',  ( 0.1565249325564390115, -0.1468220338983060036, 7.048192310558509810 ) ) ;
#3000 = CARTESIAN_POINT ( 'NONE',  ( -1.044181395669830259, -2.052854336594790219, 2.590869634085910089 ) ) ;
#3001 = EDGE_LOOP ( 'NONE', ( #726, #6898, #8837, #4793 ) ) ;
#3002 = ORIENTED_EDGE ( 'NONE', *, *, #2939, .F. ) ;
#3003 = CARTESIAN_POINT ( 'NONE',  ( 2.111627294540149080, -3.710163681423230386, 3.660877362176660377 ) ) ;
#3004 = AXIS2_PLACEMENT_3D ( 'NONE', #9172, #6218, #855 ) ;
#3005 = CARTESIAN_POINT ( 'NONE',  ( -1.248294325655370018, -5.573305084745760141, 2.704938983774309857 ) ) ;
#3006 = ORIENTED_EDGE ( 'NONE', *, *, #4825, .T. ) ;
#3007 = CARTESIAN_POINT ( 'NONE',  ( 1.202278654260740876, -0.4201271186440683758, 6.364093491318035589 ) ) ;
#3008 = EDGE_CURVE ( 'NONE', #6669, #15169, #3624, .T. ) ;
#3009 = ORIENTED_EDGE ( 'NONE', *, *, #16003, .F. ) ;
#3010 = DIRECTION ( 'NONE',  ( 1.306144734853129823E-16, -1.000000000000000000, 0.000000000000000000 ) ) ;
#3011 = CARTESIAN_POINT ( 'NONE',  ( 2.048006021857541548, -2.541908390648840665, 4.556566471620634218 ) ) ;
#3012 = CARTESIAN_POINT ( 'NONE',  ( 1.800129581279440893, -0.3355932203389832558, 2.750028594811110061 ) ) ;
#3013 = EDGE_LOOP ( 'NONE', ( #15454, #10603, #8037, #7558 ) ) ;
#3014 = CARTESIAN_POINT ( 'NONE',  ( 11.62823001646930088, 2.140775818696779709E-14, 0.5999999999998879563 ) ) ;
#3015 = ORIENTED_EDGE ( 'NONE', *, *, #9251, .T. ) ;
#3016 = DIRECTION ( 'NONE',  ( -1.000000000000000000, 1.850371707708589879E-16, 0.000000000000000000 ) ) ;
#3017 = CARTESIAN_POINT ( 'NONE',  ( 2.293398556041700065, -5.364194915254239859, 4.171956209133470317 ) ) ;
#3018 = DIRECTION ( 'NONE',  ( -1.000000000000000000, 0.000000000000000000, 0.000000000000000000 ) ) ;
#3019 = DIRECTION ( 'NONE',  ( 1.000000000000000000, 0.000000000000000000, 0.000000000000000000 ) ) ;
#3020 = EDGE_LOOP ( 'NONE', ( #940, #12994, #1646, #1971 ) ) ;
#3021 = CARTESIAN_POINT ( 'NONE',  ( -2.311987889326990064, -1.521064582324129999, 4.260161748947139948 ) ) ;
#3022 = CARTESIAN_POINT ( 'NONE',  ( -1.000000000000000000, 6.400000000000000355, 7.700000000000000178 ) ) ;
#3023 = CARTESIAN_POINT ( 'NONE',  ( 0.2739924515130530702, -2.615614131873680748, 6.734657214162127481 ) ) ;
#3024 = FACE_OUTER_BOUND ( 'NONE', #14043, .T. ) ;
#3025 = ADVANCED_FACE ( 'NONE', ( #12246 ), #17868, .F. ) ;
#3026 = ORIENTED_EDGE ( 'NONE', *, *, #3366, .F. ) ;
#3027 = ADVANCED_FACE ( 'NONE', ( #9274 ), #8089, .T. ) ;
#3028 =( GEOMETRIC_REPRESENTATION_CONTEXT ( 3 ) GLOBAL_UNCERTAINTY_ASSIGNED_CONTEXT ( ( #15484 ) ) GLOBAL_UNIT_ASSIGNED_CONTEXT ( ( #10944, #12592, #3895 ) ) REPRESENTATION_CONTEXT ( 'NONE', 'WORKASPACE' ) );
#3029 = DIRECTION ( 'NONE',  ( 1.000000000000000000, 0.000000000000000000, 0.000000000000000000 ) ) ;
#3030 = CARTESIAN_POINT ( 'NONE',  ( 0.6640878839024751956, -0.4379237288135597317, 7.269405042592523181 ) ) ;
#3031 = EDGE_CURVE ( 'NONE', #10172, #2860, #5550, .T. ) ;
#3032 = CARTESIAN_POINT ( 'NONE',  ( -1.951437470830620136, -5.057043525783970317, 3.384463041838880137 ) ) ;
#3033 = LINE ( 'NONE', #4047, #1586 ) ;
#3034 = EDGE_CURVE ( 'NONE', #10505, #12165, #6785, .T. ) ;
#3035 = DIRECTION ( 'NONE',  ( 1.643460219210440021E-31, 1.000000000000000000, 2.220446049250309876E-16 ) ) ;
#3036 = CARTESIAN_POINT ( 'NONE',  ( -2.130266475405059090, -5.255508474576275901, 3.117337770017961418 ) ) ;
#3037 = ORIENTED_EDGE ( 'NONE', *, *, #17487, .F. ) ;
#3038 = ORIENTED_EDGE ( 'NONE', *, *, #11416, .F. ) ;
#3039 = CARTESIAN_POINT ( 'NONE',  ( -0.1749999999999999889, 7.500000000000000000, 3.100000000000000089 ) ) ;
#3040 =( NAMED_UNIT ( * ) PLANE_ANGLE_UNIT ( ) SI_UNIT ( $, .RADIAN. ) );
#3041 = LINE ( 'NONE', #3118, #17614 ) ;
#3042 = VERTEX_POINT ( 'NONE', #18051 ) ;
#3043 = CARTESIAN_POINT ( 'NONE',  ( 1.256119432346080478, -1.261052534792989288, 7.037793332329536966 ) ) ;
#3044 = AXIS2_PLACEMENT_3D ( 'NONE', #13463, #16150, #7817 ) ;
#3045 = CARTESIAN_POINT ( 'NONE',  ( 0.5843165771433389555, -0.3612150962701970447, 2.403837883145309995 ) ) ;
#3046 = LINE ( 'NONE', #17460, #17066 ) ;
#3047 = CARTESIAN_POINT ( 'NONE',  ( -1.397172971746989845, -1.707370888630439953, 2.806153814454939610 ) ) ;
#3048 = FACE_OUTER_BOUND ( 'NONE', #2480, .T. ) ;
#3049 = CARTESIAN_POINT ( 'NONE',  ( -1.630481553867809907, -3.543304787045240101, 3.002862530617889547 ) ) ;
#3050 = LINE ( 'NONE', #14338, #10224 ) ;
#3051 = CARTESIAN_POINT ( 'NONE',  ( -0.4114611322411360628, -4.567989471729919870, 6.711368086473216366 ) ) ;
#3052 = ADVANCED_FACE ( 'NONE', ( #5395 ), #11036, .T. ) ;
#3053 = DIRECTION ( 'NONE',  ( 1.850371707708589879E-16, -1.000000000000000000, 0.000000000000000000 ) ) ;
#3054 = CARTESIAN_POINT ( 'NONE',  ( -1.889999999999999902, 8.500000000000000000, 0.6099999999999999867 ) ) ;
#3055 = ORIENTED_EDGE ( 'NONE', *, *, #1335, .F. ) ;
#3056 = AXIS2_PLACEMENT_3D ( 'NONE', #14047, #18183, #11089 ) ;
#3057 = DIRECTION ( 'NONE',  ( 1.000000000000000000, 0.000000000000000000, -1.480297366166879989E-15 ) ) ;
#3058 = ORIENTED_EDGE ( 'NONE', *, *, #9452, .F. ) ;
#3059 = FACE_OUTER_BOUND ( 'NONE', #610, .T. ) ;
#3060 = FACE_OUTER_BOUND ( 'NONE', #13252, .T. ) ;
#3061 = ORIENTED_EDGE ( 'NONE', *, *, #2827, .T. ) ;
#3062 = CARTESIAN_POINT ( 'NONE',  ( -2.041338374031088865, -5.519915254237295343, 4.918217215283674726 ) ) ;
#3063 = CARTESIAN_POINT ( 'NONE',  ( 2.049607015837390911, -2.429307825567371459, 6.385889905549011480 ) ) ;
#3064 = LINE ( 'NONE', #13148, #17633 ) ;
#3065 = PRESENTATION_STYLE_ASSIGNMENT (( #15757 ) ) ;
#3066 = CARTESIAN_POINT ( 'NONE',  ( 1.250000000000000000, 7.799999999999999822, 6.100000000000000533 ) ) ;
#3067 = CARTESIAN_POINT ( 'NONE',  ( -0.1914205519645679199, -4.981295943764795453, 2.049234377954000319 ) ) ;
#3068 = CARTESIAN_POINT ( 'NONE',  ( -1.899999999999999911, 11.40000000000000036, 1.600000000000000089 ) ) ;
#3069 = CARTESIAN_POINT ( 'NONE',  ( -1.899999999999999911, 7.299999999999999822, 1.600000000000000089 ) ) ;
#3070 = CARTESIAN_POINT ( 'NONE',  ( 1.962536940652990003, -2.704926408666860294, 5.998920491814760503 ) ) ;
#3071 = CARTESIAN_POINT ( 'NONE',  ( 2.041954431566909367, -3.849893411152959910, 4.912894203848615859 ) ) ;
#3072 = CARTESIAN_POINT ( 'NONE',  ( -0.7093417302541390468, -0.1646186440677969987, 6.943956659919700236 ) ) ;
#3073 = EDGE_CURVE ( 'NONE', #13656, #6275, #2245, .T. ) ;
#3074 = CARTESIAN_POINT ( 'NONE',  ( -1.850000000000000089, -5.599999999999999645, 6.899999999999999467 ) ) ;
#3075 = CARTESIAN_POINT ( 'NONE',  ( 0.3367924244280819934, 2.254758922476410188, 7.700000000000000178 ) ) ;
#3076 = VERTEX_POINT ( 'NONE', #6501 ) ;
#3077 = CARTESIAN_POINT ( 'NONE',  ( -1.991177874369409961, -3.221109627369172390, 2.945484578117480989 ) ) ;
#3078 = CARTESIAN_POINT ( 'NONE',  ( 1.980638384804650931, -0.06228813559322075172, 4.159858630563753934 ) ) ;
#3079 = CARTESIAN_POINT ( 'NONE',  ( 2.075124426334590044, -2.681638120378570189, 5.810227140144509583 ) ) ;
#3080 = ORIENTED_EDGE ( 'NONE', *, *, #16715, .T. ) ;
#3081 = LINE ( 'NONE', #5773, #1143 ) ;
#3082 = VERTEX_POINT ( 'NONE', #1311 ) ;
#3083 = CARTESIAN_POINT ( 'NONE',  ( 0.8001898266890952183, -4.129352870612411408, 6.913242401714550844 ) ) ;
#3084 = APPLICATION_PROTOCOL_DEFINITION ( 'draft international standard', 'automotive_design', 1998, #1072 ) ;
#3085 = CARTESIAN_POINT ( 'NONE',  ( -0.6640878839024662028, -5.162076271186444743, 7.269405042592523181 ) ) ;
#3086 = ORIENTED_EDGE ( 'NONE', *, *, #16604, .T. ) ;
#3087 = CARTESIAN_POINT ( 'NONE',  ( 2.500000000000000000, 11.15000000000000036, -1.135674796306499891E-15 ) ) ;
#3088 = CARTESIAN_POINT ( 'NONE',  ( 1.980638384804650931, -0.3622881355932213721, 4.159858630563753934 ) ) ;
#3089 = ORIENTED_EDGE ( 'NONE', *, *, #8247, .T. ) ;
#3090 = DIRECTION ( 'NONE',  ( 0.000000000000000000, 0.000000000000000000, 1.000000000000000000 ) ) ;
#3091 = DIRECTION ( 'NONE',  ( 0.000000000000000000, 0.000000000000000000, -1.000000000000000000 ) ) ;
#3092 = CARTESIAN_POINT ( 'NONE',  ( 0.1749999999999999889, 7.700000000000000178, 0.4000000000000000222 ) ) ;
#3093 = CARTESIAN_POINT ( 'NONE',  ( -1.079900583135680714, -2.029566048306499670, 2.953942563037710300 ) ) ;
#3094 = EDGE_CURVE ( 'NONE', #12326, #1091, #15895, .T. ) ;
#3095 = ORIENTED_EDGE ( 'NONE', *, *, #7669, .F. ) ;
#3096 = CARTESIAN_POINT ( 'NONE',  ( 1.850000000000000089, 0.7500000000000000000, 8.300000000000000711 ) ) ;
#3097 = DIRECTION ( 'NONE',  ( 0.000000000000000000, -1.000000000000000000, 2.220446049250320181E-15 ) ) ;
#3098 = ORIENTED_EDGE ( 'NONE', *, *, #10545, .F. ) ;
#3099 = CARTESIAN_POINT ( 'NONE',  ( 1.791574935211219799, -5.408686440677969998, 6.226029630577610163 ) ) ;
#3100 = CARTESIAN_POINT ( 'NONE',  ( -0.9150601050661557601, -0.1690677966101701013, 6.868218666554229301 ) ) ;
#3101 = CARTESIAN_POINT ( 'NONE',  ( -0.1471036068827911436, -0.2965485159365571777, 2.649244128781490737 ) ) ;
#3102 = EDGE_LOOP ( 'NONE', ( #10845, #13388, #5563, #11480 ) ) ;
#3103 = CARTESIAN_POINT ( 'NONE',  ( -1.000000000000000000, 6.400000000000000355, 8.300000000000000711 ) ) ;
#3104 = CARTESIAN_POINT ( 'NONE',  ( 0.8934014991060330590, -0.9854339516935011201, 6.877287176483390496 ) ) ;
#3105 = DIRECTION ( 'NONE',  ( 1.000000000000000000, 0.000000000000000000, 0.000000000000000000 ) ) ;
#3106 = CARTESIAN_POINT ( 'NONE',  ( -1.472933559740131626, -2.848497014756559143, 6.130163826706357177 ) ) ;
#3107 = CARTESIAN_POINT ( 'NONE',  ( 0.2000000000000000111, 0.1000000000000000056, 8.300000000000000711 ) ) ;
#3108 = ORIENTED_EDGE ( 'NONE', *, *, #16254, .F. ) ;
#3109 = CARTESIAN_POINT ( 'NONE',  ( 8.572527594031470232E-16, -7.000000000000000000, -4.286263797015740046E-16 ) ) ;
#3110 = CARTESIAN_POINT ( 'NONE',  ( 0.1765068388402390998, -0.4468220338983063811, 7.347961541693647902 ) ) ;
#3111 = CARTESIAN_POINT ( 'NONE',  ( -1.092567884283820012, -4.637854336594780413, 6.784476218553590066 ) ) ;
#3112 = DIRECTION ( 'NONE',  ( -0.000000000000000000, 1.000000000000000000, 0.000000000000000000 ) ) ;
#3113 = LINE ( 'NONE', #8674, #14503 ) ;
#3114 = CARTESIAN_POINT ( 'NONE',  ( 2.286166334984490067, -5.086440677966099777, 5.258525443163859947 ) ) ;
#3115 = ORIENTED_EDGE ( 'NONE', *, *, #11653, .F. ) ;
#3116 = ORIENTED_EDGE ( 'NONE', *, *, #5180, .T. ) ;
#3117 = CARTESIAN_POINT ( 'NONE',  ( 1.889999999999999902, 7.900000000000000355, 2.872493252184739990E-16 ) ) ;
#3118 = CARTESIAN_POINT ( 'NONE',  ( 1.800000000000000044, 11.40000000000000036, 1.600000000000000089 ) ) ;
#3119 = ORIENTED_EDGE ( 'NONE', *, *, #3073, .T. ) ;
#3120 = CARTESIAN_POINT ( 'NONE',  ( 2.174104834890520976, -1.144611093351550091, 6.221966445066246187 ) ) ;
#3121 = EDGE_CURVE ( 'NONE', #10238, #5712, #2715, .T. ) ;
#3122 = CARTESIAN_POINT ( 'NONE',  ( 0.2254033459420760055, -0.6247245358507570456, 2.348900562125120217 ) ) ;
#3123 = FACE_OUTER_BOUND ( 'NONE', #3380, .T. ) ;
#3124 = EDGE_CURVE ( 'NONE', #9612, #786, #7242, .T. ) ;
#3125 = CARTESIAN_POINT ( 'NONE',  ( -0.9719602541832299547, -2.755343861603410271, 6.843370931913550059 ) ) ;
#3126 = CARTESIAN_POINT ( 'NONE',  ( 0.5677251586959709551, -5.311531839079339790, 2.399563163165729929 ) ) ;
#3127 = CARTESIAN_POINT ( 'NONE',  ( 2.629224451638851434, -0.9583047870452394701, 4.339039509243856507 ) ) ;
#3128 = DIRECTION ( 'NONE',  ( 0.000000000000000000, -1.000000000000000000, 0.000000000000000000 ) ) ;
#3129 = CARTESIAN_POINT ( 'NONE',  ( -1.886482464143629967, -5.010466949207390108, 3.890008792968694618 ) ) ;
#3130 = CARTESIAN_POINT ( 'NONE',  ( 0.2750000000000004663, 2.299999999999999822, 7.599999999999999645 ) ) ;
#3131 = CARTESIAN_POINT ( 'NONE',  ( -0.4974685680287780354, -0.4601694915254240237, 7.000224381598740386 ) ) ;
#3132 = CARTESIAN_POINT ( 'NONE',  ( -2.500000000000000000, 11.29999999999999893, 1.600000000000000089 ) ) ;
#3133 = EDGE_LOOP ( 'NONE', ( #14486, #8062, #7965 ) ) ;
#3134 = VECTOR ( 'NONE', #15451, 1000.000000000000000 ) ;
#3135 = ORIENTED_EDGE ( 'NONE', *, *, #9697, .T. ) ;
#3136 = CARTESIAN_POINT ( 'NONE',  ( 11.62823001646920140, 2.147437156844530270E-14, -1.123545700920659934E-13 ) ) ;
#3137 = EDGE_CURVE ( 'NONE', #410, #4501, #17126, .T. ) ;
#3138 = ORIENTED_EDGE ( 'NONE', *, *, #11966, .F. ) ;
#3139 = CARTESIAN_POINT ( 'NONE',  ( 1.795861365445541091, -5.350847457627126325, 3.705232155007893713 ) ) ;
#3140 = CARTESIAN_POINT ( 'NONE',  ( 0.6015868932280445947, -2.592325843585391532, 7.284803068494412948 ) ) ;
#3141 = EDGE_CURVE ( 'NONE', #11906, #17304, #16772, .T. ) ;
#3142 = CARTESIAN_POINT ( 'NONE',  ( -3.061616997868380553E-17, 5.318248954186070243, 6.899999999999999467 ) ) ;
#3143 = DIRECTION ( 'NONE',  ( 0.000000000000000000, -1.000000000000000000, -4.440892098500630106E-16 ) ) ;
#3144 = EDGE_CURVE ( 'NONE', #11596, #8415, #4450, .T. ) ;
#3145 = CARTESIAN_POINT ( 'NONE',  ( -1.408343819019460219E-16, 7.000000000000000000, 5.100000000000000533 ) ) ;
#3146 = AXIS2_PLACEMENT_3D ( 'NONE', #12060, #17680, #2440 ) ;
#3147 = VECTOR ( 'NONE', #16065, 1000.000000000000000 ) ;
#3148 = DIRECTION ( 'NONE',  ( 1.000000000000000000, 0.000000000000000000, 0.000000000000000000 ) ) ;
#3149 = CARTESIAN_POINT ( 'NONE',  ( -1.289999999999999813, 4.099999999999999645, 3.000000000000001776 ) ) ;
#3150 = CARTESIAN_POINT ( 'NONE',  ( -0.5320716618283710675, -3.007674156414609890, 6.992519451207139802 ) ) ;
#3151 = CARTESIAN_POINT ( 'NONE',  ( -0.4365326870213908639, -4.269082600342137823, 6.706076034398992469 ) ) ;
#3152 = CARTESIAN_POINT ( 'NONE',  ( 0.5137283630188955730, -0.1379237288135599648, 6.687652957477222770 ) ) ;
#3153 = ADVANCED_FACE ( 'NONE', ( #15410 ), #14356, .T. ) ;
#3154 = CARTESIAN_POINT ( 'NONE',  ( -0.2335786437626909962, 6.450000000000000178, 1.958578643762689753 ) ) ;
#3155 = VECTOR ( 'NONE', #583, 1000.000000000000000 ) ;
#3156 = VECTOR ( 'NONE', #4485, 1000.000000000000000 ) ;
#3157 = CARTESIAN_POINT ( 'NONE',  ( -2.500000000000000000, 3.996802888650570054E-16, 9.955530934770520091 ) ) ;
#3158 = ORIENTED_EDGE ( 'NONE', *, *, #5156, .F. ) ;
#3159 = CARTESIAN_POINT ( 'NONE',  ( -1.256119432346030962, -4.338947465207014353, 7.037793332329566276 ) ) ;
#3160 = CARTESIAN_POINT ( 'NONE',  ( 0.5664586606772286093, -0.3133474576271193524, 2.726727161522279452 ) ) ;
#3161 = CARTESIAN_POINT ( 'NONE',  ( 0.7678268402137939930, -2.867944426684879922, 6.924676972266129660 ) ) ;
#3162 = ORIENTED_EDGE ( 'NONE', *, *, #4278, .T. ) ;
#3163 = ORIENTED_EDGE ( 'NONE', *, *, #10051, .F. ) ;
#3164 = DIRECTION ( 'NONE',  ( 1.233581138472399909E-16, 6.167905692361979821E-17, -1.000000000000000000 ) ) ;
#3165 = VECTOR ( 'NONE', #5158, 1000.000000000000000 ) ;
#3166 = ORIENTED_EDGE ( 'NONE', *, *, #15506, .F. ) ;
#3167 = VECTOR ( 'NONE', #8151, 1000.000000000000000 ) ;
#3168 = CARTESIAN_POINT ( 'NONE',  ( 0.4201920264139499817, -3.477280798540341333, 2.384360920086630031 ) ) ;
#3169 = SHAPE_DEFINITION_REPRESENTATION ( #4014, #4513 ) ;
#3170 = CARTESIAN_POINT ( 'NONE',  ( -1.407651048079459288, -5.573305084745765470, 2.450250343405070641 ) ) ;
#3171 = AXIS2_PLACEMENT_3D ( 'NONE', #15075, #985, #5050 ) ;
#3172 = EDGE_CURVE ( 'NONE', #8719, #2042, #11318, .T. ) ;
#3173 = ORIENTED_EDGE ( 'NONE', *, *, #17275, .T. ) ;
#3174 = FACE_OUTER_BOUND ( 'NONE', #3259, .T. ) ;
#3175 = VECTOR ( 'NONE', #4358, 1000.000000000000000 ) ;
#3176 = CARTESIAN_POINT ( 'NONE',  ( 2.340070819011249803, -0.3800847457627120063, 4.950151441910540129 ) ) ;
#3177 = MECHANICAL_DESIGN_GEOMETRIC_PRESENTATION_REPRESENTATION (  '', ( #16775 ), #15639 ) ;
#3178 = ORIENTED_EDGE ( 'NONE', *, *, #3951, .T. ) ;
#3179 = AXIS2_PLACEMENT_3D ( 'NONE', #14283, #15850, #1604 ) ;
#3180 = CARTESIAN_POINT ( 'NONE',  ( -0.6500000000000000222, 6.450000000000000178, 2.699264068711930253 ) ) ;
#3181 = PLANE ( 'NONE',  #3799 ) ;
#3182 = CARTESIAN_POINT ( 'NONE',  ( -0.8259795455965642796, -3.054250732991181216, 6.579537079411896805 ) ) ;
#3183 = CARTESIAN_POINT ( 'NONE',  ( 2.560337424259670591, -0.3622881355932213721, 4.001768473655590519 ) ) ;
#3184 = AXIS2_PLACEMENT_3D ( 'NONE', #9668, #2741, #4291 ) ;
#3185 = ORIENTED_EDGE ( 'NONE', *, *, #7481, .F. ) ;
#3186 = AXIS2_PLACEMENT_3D ( 'NONE', #9689, #11361, #8490 ) ;
#3187 = DIRECTION ( 'NONE',  ( 0.000000000000000000, -1.000000000000000000, 0.000000000000000000 ) ) ;
#3188 = ADVANCED_FACE ( 'NONE', ( #9921 ), #17034, .T. ) ;
#3189 = ORIENTED_EDGE ( 'NONE', *, *, #1049, .F. ) ;
#3190 = VECTOR ( 'NONE', #17756, 1000.000000000000000 ) ;
#3191 = CARTESIAN_POINT ( 'NONE',  ( -2.500000000000000000, 2.799999999999999822, 0.5999999999999999778 ) ) ;
#3192 = CARTESIAN_POINT ( 'NONE',  ( -2.041338374031088865, -5.519915254237295343, 4.918217215283674726 ) ) ;
#3193 = VECTOR ( 'NONE', #7406, 1000.000000000000000 ) ;
#3194 = CARTESIAN_POINT ( 'NONE',  ( -1.925796468768789405, -0.1957627118644069963, 6.052706598917718672 ) ) ;
#3195 = CARTESIAN_POINT ( 'NONE',  ( 2.247144151254821143, -3.985782264522713447, 3.288101683376901452 ) ) ;
#3196 = EDGE_CURVE ( 'NONE', #1235, #13357, #16484, .T. ) ;
#3197 = EDGE_LOOP ( 'NONE', ( #10194, #6253, #7492, #4463 ) ) ;
#3198 = VECTOR ( 'NONE', #13482, 1000.000000000000000 ) ;
#3199 = CARTESIAN_POINT ( 'NONE',  ( -0.7678268402137429227, -2.732055573315119723, 6.924676972266150088 ) ) ;
#3200 = DIRECTION ( 'NONE',  ( -1.000000000000000000, 6.161988852941170860E-64, 6.123233995736769734E-17 ) ) ;
#3201 = VECTOR ( 'NONE', #3586, 1000.000000000000000 ) ;
#3202 = CARTESIAN_POINT ( 'NONE',  ( -1.893291846171410331, -2.941650167909708458, 5.493944474033886749 ) ) ;
#3203 = AXIS2_PLACEMENT_3D ( 'NONE', #4707, #10928, #13882 ) ;
#3204 = CARTESIAN_POINT ( 'NONE',  ( -1.850000000000000089, -5.599999999999999645, 2.799999999999999822 ) ) ;
#3205 = CARTESIAN_POINT ( 'NONE',  ( 0.5000000000000000000, 4.631370849898480024, 5.100000000000000533 ) ) ;
#3206 = ORIENTED_EDGE ( 'NONE', *, *, #9000, .T. ) ;
#3207 = VECTOR ( 'NONE', #17429, 1000.000000000000000 ) ;
#3208 = LINE ( 'NONE', #14319, #543 ) ;
#3209 = DIRECTION ( 'NONE',  ( 1.110223024625159992E-16, 0.000000000000000000, -1.000000000000000000 ) ) ;
#3210 = CARTESIAN_POINT ( 'NONE',  ( -1.899999999999999911, 9.199999999999999289, 1.600000000000000089 ) ) ;
#3211 = FACE_OUTER_BOUND ( 'NONE', #15985, .T. ) ;
#3212 = CARTESIAN_POINT ( 'NONE',  ( -1.747582379783008788, -5.184322033898315141, 6.697200745122486865 ) ) ;
#3213 = VERTEX_POINT ( 'NONE', #10109 ) ;
#3214 = VERTEX_POINT ( 'NONE', #14275 ) ;
#3215 = CARTESIAN_POINT ( 'NONE',  ( 2.500000000000000000, 2.799999999999999822, 1.600000000000000089 ) ) ;
#3216 = SHAPE_REPRESENTATION_RELATIONSHIP ( 'NONE' , 'NONE' ,  #2027, #3778 ) ;
#3217 = VECTOR ( 'NONE', #10695, 1000.000000000000000 ) ;
#3218 = CARTESIAN_POINT ( 'NONE',  ( 1.699999999999999956, 9.299999999999998934, 7.599999999999999645 ) ) ;
#3219 = CIRCLE ( 'NONE', #12088, 0.04999999999999969746 ) ;
#3220 = VERTEX_POINT ( 'NONE', #13993 ) ;
#3221 = DIRECTION ( 'NONE',  ( -1.000000000000000000, -4.433365283261159518E-17, -1.187916647401989926E-17 ) ) ;
#3222 = CARTESIAN_POINT ( 'NONE',  ( -0.2266049403550400299, -2.146007489747939090, 2.055805624768001216 ) ) ;
#3223 = LINE ( 'NONE', #8955, #12945 ) ;
#3224 = DIRECTION ( 'NONE',  ( 1.000000000000000000, 4.037174635000579950E-16, 0.000000000000000000 ) ) ;
#3225 = CARTESIAN_POINT ( 'NONE',  ( 0.7435598031058590074, -2.569037555297100095, 6.932904947974519949 ) ) ;
#3226 = EDGE_CURVE ( 'NONE', #1639, #14807, #10022, .T. ) ;
#3227 = CARTESIAN_POINT ( 'NONE',  ( 1.315859850362970151, -5.328211948015590060, 2.737664967889629875 ) ) ;
#3228 =( BOUNDED_SURFACE ( )  B_SPLINE_SURFACE ( 3, 3, ( 
 ( #4196, #9856, #5411, #16794, #7088, #6977, #12625, #15514, #11337, #8288, #4284, #14537, #18250, #4611, #15332, #15603, #1246, #4008, #14100, #5600, #16888, #2639, #11244, #48, #8462, #11138, #5691, #4107, #10269, #6802, #12450, #2917, #8562, #15940, #13929, #6888, #14208, #12536, #18148, #9763, #15428, #1770, #7417, #377, #4795, #16199, #17475, #13517, #7681, #10446, #14813, #16383, #13418, #1855, #11939, #16027, #16107, #10535, #10649, #14620, #7584, #4887, #555, #3403, #14910, #8972, #6199, #3689, #4995, #11857, #7865, #13325, #6475, #3508, #833, #13147, #459, #10362, #4713, #2124, #6101, #9051, #9336, #732, #12135, #13236, #3327, #7774, #6280, #17755, #16294, #5086, #1934, #6367, #14708, #2026, #641, #10736, #12034, #7500, #17655, #17556, #3600, #9152, #9247, #2219, #11764, #17392, #3788, #18195, #9446, #15380, #15109, #1289, #2421, #13785, #9620, #17937, #6849, #10829, #5279, #16472, #2321, #8335, #13885, #8149, #12579, #1019, #13968, #8069, #15194, #6756, #13709, #5457, #12222, #6932, #1201, #15006, #6569, #17838, #930, #15280, #7971, #16578, #2589, #4150, #2502, #3883, #5176, #1109, #18110, #12494, #13619, #3968, #5552, #12406, #11098, #6656, #12314, #16745, #11196, #18028, #16839, #10930, #9535, #5375, #11013, #8240, #16661, #4058, #9713, #12857, #11640, #13037, #1567, #4326, #4425, #168, #7037, #14425, #9992, #15466, #14161, #5816, #15738, #7212, #5911, #3 ),
 ( #17011, #15816, #7398, #14250, #9898, #9809, #17101, #8773, #5732, #5997, #2862, #12772, #16928, #15656, #1651, #10086, #3120, #358, #17185, #85, #11466, #3043, #2775, #14056, #1373, #7138, #12681, #5644, #8683, #2965, #11287, #15556, #4237, #8510, #1480, #14330, #12946, #11552, #8606, #273, #4507, #9127, #7842, #2099, #7750, #6082, #17458, #4776, #15911, #10427, #16090, #4867, #17366, #14599, #16011, #2002, #6259, #7659, #13303, #3222, #8869, #7564, #1915, #622, #10344, #6177, #17627, #11732, #3311, #806, #13396, #8954, #10622, #3385, #9220, #11919, #16270, #14518, #1837, #13130, #7480, #10512, #442, #11835, #6447, #16176, #3573, #13211, #4691, #3481, #9030, #2198, #710, #14884, #530, #14783, #14686, #17538, #6345, #13489, #12008, #12114, #4966, #4583, #10242, #6633, #3761, #10804, #12290, #6548, #17817, #8315, #2398, #18091, #8047, #9688, #13688, #9515, #12387, #996, #9600, #17910, #5253, #10910, #16360, #5438, #16643, #15174, #15360, #2483, #11079, #8128, #13763, #6732, #5351, #10995, #3947, #15256, #2561, #8216, #13864, #1270, #1181, #6914, #6829, #12473, #3666, #6411, #9488, #15060, #17883, #17703, #2368, #1062, #3730, #882, #6704, #12175, #1158, #9663, #7815, #5329, #12361, #11053, #13461, #12452, #5221, #9290, #14952, #778, #10690, #17983, #2262, #17793, #5129, #16529, #10779, #13838, #970, #16425, #2459, #5034, #10974, #7915, #16620, #13565, #9392, #3923 ),
 ( #6607, #9576, #15235, #8189, #6805, #18069, #347, #5984, #11626, #9017, #14411, #10332, #7645, #16253, #14587, #15996, #17255, #7549, #4853, #609, #4572, #16076, #14768, #516, #10499, #10229, #15899, #6247, #2082, #8941, #13379, #17610, #694, #7470, #4949, #16158, #11821, #14506, #1827, #17445, #10602, #13118, #6164, #3299, #3372, #4763, #429, #6068, #10414, #11717, #17350, #3461, #9110, #4679, #17994, #12096, #14966, #8115, #2549, #8030, #9204, #2383, #5140, #3932, #13851, #13670, #3649, #11064, #10893, #8202, #17803, #18081, #2277, #6532, #10701, #16437, #13752, #3849, #15245, #9586, #10985, #12186, #982, #12276, #1169, #6815, #14868, #893, #13473, #5427, #15157, #15073, #17715, #9299, #12463, #7931, #16344, #16542, #6718, #5341, #6618, #13579, #17896, #1074, #3558, #12373, #16632, #5047, #3743, #9407, #2183, #5236, #9503, #2468, #10791, #7826, #789, #6427, #3077, #4459, #10116, #9675, #2652, #2747, #9777, #15768, #5512, #14364, #15347, #14027, #17300, #12985, #1786, #11155, #13941, #7341, #11257, #13072, #4536, #14465, #6902, #1690, #16807, #15439, #1341, #7430, #306, #390, #11584, #16901, #5945, #6995, #4120, #8392, #12642, #12552, #18161, #6029, #18267, #8814, #5614, #11675, #8720, #17215, #10189, #15853, #3159, #4628, #16708, #4020, #1259, #8303, #13814, #8088, #12777, #954, #15559, #9364, #15130, #6591, #15216, #2441, #3817, #12340, #1138, #16407, #12686, #11380 ),
 ( #13729, #2244, #12245, #10952, #2523, #6682, #11293, #5111, #7997, #7042, #14166, #1045, #7891, #17961, #16504, #2866, #7141, #5307, #15034, #4330, #3903, #1485, #10858, #17014, #13644, #17866, #3712, #9467, #8, #8170, #8516, #92, #4240, #5205, #16601, #9558, #5736, #14934, #13542, #5649, #6500, #860, #16930, #9902, #10763, #2347, #12161, #17777, #4430, #17269, #13133, #11737, #8776, #3047, #14429, #14521, #13214, #7485, #445, #11470, #4511, #10162, #11557, #8687, #15915, #14334, #8958, #17461, #9996, #6086, #8873, #535, #15661, #1918, #1754, #5819, #17105, #2970, #172, #1841, #10089, #7301, #12950, #6000, #276, #3315, #15820, #5916, #4589, #6183, #3225, #8611, #7402, #15741, #17188, #362, #17372, #1654, #3125, #13040, #11643, #10248, #4695, #10348, #16014, #11839, #14603, #7568, #14254, #1572, #7218, #12861, #10807, #16093, #3389, #13309, #7663, #5065, #9034, #6348, #998, #16365, #16453, #16179, #625, #10716, #9225, #2402, #913, #3765, #6262, #3669, #3485, #14788, #12012, #9426, #9316, #15090, #2298, #14888, #14987, #17632, #9130, #2103, #4970, #11924, #17541, #8049, #4870, #5157, #10517, #13690, #7754, #3577, #17737, #13399, #7951, #714, #10626, #16274, #10431, #6635, #13598, #2201, #12293, #7845, #4780, #13495, #810, #6451, #6551, #12117, #12203, #17820, #14690, #2007, #15452, #14137, #6832, #4221, #2485, #14040, #12389, #3864, #6916, #12476, #9690, #15176 ),
 ( #18094, #9881, #8130, #1356, #18008, #9518, #12564, #5441, #15362, #13765, #11081, #5528, #1183, #16646, #11171, #3950, #16912, #7116, #17913, #7012, #16821, #2842, #5256, #15541, #2663, #6734, #5355, #10912, #10997, #4133, #9602, #15259, #2564, #13954, #8218, #11271, #16723, #13866, #18176, #1461, #9791, #16556, #8318, #4036, #12661, #18284, #5627, #8491, #153, #15798, #11446, #14315, #7465, #1551, #17080, #8935, #15890, #4409, #424, #5893, #17342, #14404, #6060, #5716, #11362, #2946, #15638, #13019, #16995, #1637, #14583, #5979, #11709, #5799, #8586, #342, #17170, #10328, #8853, #4674, #14232, #11620, #10068, #15721, #7281, #15989, #17248, #3292, #10223, #4488, #4567, #12928, #3023, #8665, #254, #7198, #12839, #1899, #11536, #13113, #10142, #12756, #3106, #8754, #7381, #1731, #3202, #14499, #1821, #70, #4309, #9974, #6418, #685, #5132, #11900, #7919, #1977, #7728, #17519, #7818, #13372, #14761, #4940, #6241, #6520, #15064, #13187, #10693, #12087, #10783, #505, #17795, #17601, #3367, #9010, #6156, #16068, #17706, #14661, #4846, #10492, #3550, #16151, #885, #6323, #3452, #2176, #3734, #5037, #11814, #10592, #7638, #9100, #16245, #16336, #13284, #602, #9197, #2073, #11986, #2265, #14861, #13464, #9396, #3640, #14955, #13570, #12178, #16428, #17439, #4757, #10407, #13661, #10880, #5225, #2646, #6610, #3927, #16895, #13934, #14020, #13746, #16533, #8296, #6809, #18259, #16800 ),
 ( #1336, #1252, #12632, #18155, #12456, #6895, #9580, #1065, #6709, #15239, #3841, #9493, #5606, #15151, #2740, #2462, #6984, #8109, #1163, #15339, #5333, #12545, #12366, #10978, #17987, #8020, #8385, #5501, #13842, #11251, #16626, #4203, #2541, #8193, #18072, #11146, #5420, #11058, #16704, #4114, #4013, #9771, #9862, #9667, #2372, #15434, #973, #12268, #17887, #4471, #10047, #7265, #12735, #15701, #3093, #17062, #14214, #8736, #15521, #323, #14380, #407, #2825, #7448, #12908, #11343, #16978, #8471, #5699, #1708, #4290, #12823, #136, #11521, #5784, #8835, #3011, #11426, #10128, #11693, #7360, #14109, #233, #9949, #4389, #5874, #5961, #15613, #2924, #17149, #1534, #8653, #10204, #8568, #7183, #17321, #11601, #14299, #3182, #1622, #1805, #15784, #14484, #1437, #7096, #13001, #53, #17231, #4550, #15871, #4651, #13090, #6047, #3352, #488, #16225, #14743, #7894, #6393, #3625, #6135, #10569, #8995, #1957, #11884, #9275, #3533, #2246, #7799, #2057, #9180, #17504, #14644, #7617, #4823, #11799, #17420, #13546, #4740, #10675, #10390, #14936, #16054, #9081, #4913, #13265, #2158, #586, #6225, #10474, #15973, #16320, #14843, #3429, #863, #16131, #6503, #7711, #13355, #669, #13447, #6307, #11965, #17580, #759, #12063, #17683, #12163, #5020, #17779, #13171, #10309, #3276, #14565, #8917, #1879, #7527, #2351, #5310, #11037, #6686, #3821, #16685, #9471, #4088, #12609, #15132, #3993 ),
 ( #5483, #15412, #9560, #5208, #5113, #12434, #9747, #1047, #1313, #16507, #8090, #12247, #17964, #15314, #5397, #16773, #11125, #12520, #13731, #15219, #13817, #2716, #8361, #10766, #2443, #15038, #6960, #9647, #16605, #13646, #10860, #13994, #12342, #17869, #18052, #8275, #6874, #3905, #10956, #2525, #2624, #16409, #13916, #1229, #6593, #8172, #1141, #3714, #6786, #18133, #9366, #8000, #956, #11320, #15683, #1601, #2993, #8633, #16871, #4179, #2897, #9923, #14278, #5676, #10024, #7072, #8714, #15492, #5938, #17128, #18228, #9838, #2801, #8446, #202, #5582, #1511, #5846, #7425, #5762, #7164, #14080, #17036, #3070, #10111, #11226, #7244, #11576, #11404, #14358, #1408, #12714, #4453, #17208, #116, #4531, #3150, #10183, #16956, #15848, #11497, #12885, #31, #4264, #15763, #1777, #8806, #1682, #12802, #7331, #12977, #15585, #14458, #4361, #8546, #14193, #299, #6284, #4800, #9156, #17480, #10653, #14819, #6373, #8893, #13334, #6109, #4717, #14624, #12040, #11944, #5002, #10542, #10451, #17561, #1939, #11772, #17399, #7591, #14542, #1858, #16300, #7505, #13424, #465, #17662, #10367, #11863, #7688, #16032, #4892, #3332, #8977, #13241, #385, #738, #16204, #6207, #3606, #563, #9256, #16112, #3409, #9058, #3513, #14714, #2033, #2133, #14914, #2223, #13065, #6025, #11670, #17293, #15949, #4621, #10280, #3249, #15200, #2428, #17941, #5091, #8073, #13794, #9453, #6574, #1119, #12228 ) ),
 .UNSPECIFIED., .T., .F., .F. ) 
 B_SPLINE_SURFACE_WITH_KNOTS ( ( 4, 3, 4 ),
 ( 4, 1, 1, 1, 1, 1, 1, 1, 1, 1, 1, 1, 1, 1, 1, 1, 1, 1, 1, 1, 1, 1, 1, 1, 1, 1, 1, 1, 1, 1, 1, 1, 1, 1, 1, 1, 1, 1, 1, 1, 1, 1, 1, 1, 1, 1, 1, 1, 1, 1, 1, 1, 1, 1, 1, 1, 1, 1, 1, 1, 1, 1, 1, 1, 1, 1, 1, 1, 1, 1, 1, 1, 1, 1, 1, 1, 1, 1, 1, 1, 1, 1, 1, 1, 1, 1, 1, 1, 1, 1, 1, 1, 1, 1, 1, 1, 1, 1, 1, 1, 1, 1, 1, 1, 1, 1, 1, 1, 1, 1, 1, 1, 1, 1, 1, 1, 1, 1, 1, 1, 1, 1, 1, 1, 1, 1, 1, 1, 1, 1, 1, 1, 1, 1, 1, 1, 1, 1, 1, 1, 1, 1, 1, 1, 1, 1, 1, 1, 1, 1, 1, 1, 1, 1, 1, 1, 1, 1, 1, 1, 1, 1, 1, 1, 1, 1, 1, 1, 1, 1, 1, 1, 1, 1, 1, 1, 1, 1, 1, 1, 1, 1, 1, 1, 1, 4 ),
 ( 0.000000000000000000, 3.141592653589790007, 6.283185307179590673 ),
 ( 0.7853981633974479459, 0.8787968639095770085, 0.9721955644217059600, 1.065594264933839908, 1.158992965445959866, 1.252391665958090039, 1.345790366470219990, 1.439189066982349940, 1.532587767494480113, 1.625986468006610064, 1.719385168518740015, 1.812783869030869965, 1.906182569543000138, 1.999581270055129867, 2.092979970567249826, 2.186378671079379998, 2.279777371591510171, 2.373176072103639900, 2.466574772615769628, 2.559973473127900245, 2.653372173640029974, 2.746770874152160147, 2.840169574664289875, 2.933568275176409834, 3.026966975688540007, 3.120365676200670180, 3.213764376712799908, 3.307163077224930081, 3.400561777737059810, 3.493960478249190427, 3.587359178761320155, 3.680757879273439670, 3.774156579785570287, 3.867555280297700016, 3.960953980809830188, 4.054352681321960361, 4.147751381834090090, 4.241150082346219818, 4.334548782858350435, 4.427947483370480164, 4.521346183882600123, 4.614744884394729851, 4.708143584906859580, 4.801542285418989309, 4.894940985931119926, 4.988339686443250542, 5.081738386955380271, 5.175137087467510000, 5.268535787979639728, 5.361934488491760575, 5.455333189003890304, 5.548731889516020033, 5.642130590028149761, 5.735529290540279490, 5.828927991052410107, 5.922326691564539836, 6.015725392076670452, 6.109124092588789523, 6.202522793100920140, 6.295921493613049869, 6.389320194125180485, 6.482718894637310214, 6.576117595149439943, 6.669516295661569671, 6.762914996173699400, 6.856313696685830017, 6.949712397197949976, 7.043111097710079704, 7.136509798222209433, 7.229908498734340050, 7.323307199246470667, 7.416705899758600395, 7.510104600270730124, 7.603503300782859853, 7.696902001294989581, 7.790300701807110428, 7.883699402319240157, 7.977098102831369886, 8.070496803343500503, 8.163895503855631119, 8.257294204367759960, 8.350692904879890577, 8.444091605392019417, 8.537490305904139376, 8.630889006416269993, 8.724287706928398833, 8.817686407440529450, 8.911085107952660067, 9.004483808464788908, 9.097882508976921301, 9.191281209489050141, 9.284679910001178982, 9.378078610513298941, 9.471477311025429557, 9.564876011537560174, 9.658274712049690791, 9.751673412561819632, 9.845072113073950248, 9.938470813586080865, 10.03186951409819905, 10.12526821461029947, 10.21866691512249936, 10.31206561563459978, 10.40546431614669842, 10.49886301665890009, 10.59226171717100051, 10.68566041768310093, 10.77905911819519957, 10.87245781870739947, 10.96585651921949989, 11.05925521973160031, 11.15265392024380020, 11.24605262075590062, 11.33945132126800104, 11.43285002178009968, 11.52624872229229958, 11.61964742280439999, 11.71304612331650041, 11.80644482382869853, 11.89984352434079895, 11.99324222485290115, 12.08664092536500156, 12.18003962587719968, 12.27343832638930010, 12.36683702690140052, 12.46023572741360042, 12.55363442792569906, 12.64703312843779948, 12.74043182894989990, 12.83383052946209979, 12.92722922997419843, 13.02062793048630063, 13.11402663099850052, 13.20742533151059916, 13.30082403202269958, 13.39422273253480000, 13.48762143304700167, 13.58102013355910032, 13.67441883407120073, 13.76781753458340063, 13.86121623509549927, 13.95461493560759969, 14.04801363611970011, 14.14141233663190000, 14.23481103714399865, 14.32820973765609907, 14.42160843816829896, 14.51500713868040116, 14.60840583919249980, 14.70180453970460022, 14.79520324021680011, 14.88860194072889875, 14.98200064124100095, 15.07539934175320084, 15.16879804226530126, 15.26219674277739990, 15.35559544328959980, 15.44899414380170022, 15.54239284431380064, 15.63579154482589928, 15.72919024533809917, 15.82258894585019959, 15.91598764636230001, 16.00938634687449991, 16.10278504738660033, 16.19618374789869719, 16.28958244841080116, 16.38298114892299751, 16.47637984943510148, 16.56977854994720190, 16.66317725045940179, 16.75657595097149866, 16.84997465148359908, 16.94337335199570305, 17.03677205250789939, 17.13017075301999981, 17.22356945353210023, 17.31696815404430012, 17.41036685455640054, 17.50376555506850096, 17.59716425558059782, 17.69056295609280127, 17.78396165660489814, 17.87736035711699856, 17.97075905762920200, 18.06415775814129887 ),
 .UNSPECIFIED. ) 
 GEOMETRIC_REPRESENTATION_ITEM ( )  RATIONAL_B_SPLINE_SURFACE ( (
 ( 1.000000000000000000, 1.000000000000000000, 1.000000000000000000, 1.000000000000000000, 1.000000000000000000, 1.000000000000000000, 1.000000000000000000, 1.000000000000000000, 1.000000000000000000, 1.000000000000000000, 1.000000000000000000, 1.000000000000000000, 1.000000000000000000, 1.000000000000000000, 1.000000000000000000, 1.000000000000000000, 1.000000000000000000, 1.000000000000000000, 1.000000000000000000, 1.000000000000000000, 1.000000000000000000, 1.000000000000000000, 1.000000000000000000, 1.000000000000000000, 1.000000000000000000, 1.000000000000000000, 1.000000000000000000, 1.000000000000000000, 1.000000000000000000, 1.000000000000000000, 1.000000000000000000, 1.000000000000000000, 1.000000000000000000, 1.000000000000000000, 1.000000000000000000, 1.000000000000000000, 1.000000000000000000, 1.000000000000000000, 1.000000000000000000, 1.000000000000000000, 1.000000000000000000, 1.000000000000000000, 1.000000000000000000, 1.000000000000000000, 1.000000000000000000, 1.000000000000000000, 1.000000000000000000, 1.000000000000000000, 1.000000000000000000, 1.000000000000000000, 1.000000000000000000, 1.000000000000000000, 1.000000000000000000, 1.000000000000000000, 1.000000000000000000, 1.000000000000000000, 1.000000000000000000, 1.000000000000000000, 1.000000000000000000, 1.000000000000000000, 1.000000000000000000, 1.000000000000000000, 1.000000000000000000, 1.000000000000000000, 1.000000000000000000, 1.000000000000000000, 1.000000000000000000, 1.000000000000000000, 1.000000000000000000, 1.000000000000000000, 1.000000000000000000, 1.000000000000000000, 1.000000000000000000, 1.000000000000000000, 1.000000000000000000, 1.000000000000000000, 1.000000000000000000, 1.000000000000000000, 1.000000000000000000, 1.000000000000000000, 1.000000000000000000, 1.000000000000000000, 1.000000000000000000, 1.000000000000000000, 1.000000000000000000, 1.000000000000000000, 1.000000000000000000, 1.000000000000000000, 1.000000000000000000, 1.000000000000000000, 1.000000000000000000, 1.000000000000000000, 1.000000000000000000, 1.000000000000000000, 1.000000000000000000, 1.000000000000000000, 1.000000000000000000, 1.000000000000000000, 1.000000000000000000, 1.000000000000000000, 1.000000000000000000, 1.000000000000000000, 1.000000000000000000, 1.000000000000000000, 1.000000000000000000, 1.000000000000000000, 1.000000000000000000, 1.000000000000000000, 1.000000000000000000, 1.000000000000000000, 1.000000000000000000, 1.000000000000000000, 1.000000000000000000, 1.000000000000000000, 1.000000000000000000, 1.000000000000000000, 1.000000000000000000, 1.000000000000000000, 1.000000000000000000, 1.000000000000000000, 1.000000000000000000, 1.000000000000000000, 1.000000000000000000, 1.000000000000000000, 1.000000000000000000, 1.000000000000000000, 1.000000000000000000, 1.000000000000000000, 1.000000000000000000, 1.000000000000000000, 1.000000000000000000, 1.000000000000000000, 1.000000000000000000, 1.000000000000000000, 1.000000000000000000, 1.000000000000000000, 1.000000000000000000, 1.000000000000000000, 1.000000000000000000, 1.000000000000000000, 1.000000000000000000, 1.000000000000000000, 1.000000000000000000, 1.000000000000000000, 1.000000000000000000, 1.000000000000000000, 1.000000000000000000, 1.000000000000000000, 1.000000000000000000, 1.000000000000000000, 1.000000000000000000, 1.000000000000000000, 1.000000000000000000, 1.000000000000000000, 1.000000000000000000, 1.000000000000000000, 1.000000000000000000, 1.000000000000000000, 1.000000000000000000, 1.000000000000000000, 1.000000000000000000, 1.000000000000000000, 1.000000000000000000, 1.000000000000000000, 1.000000000000000000, 1.000000000000000000, 1.000000000000000000, 1.000000000000000000, 1.000000000000000000, 1.000000000000000000, 1.000000000000000000, 1.000000000000000000, 1.000000000000000000, 1.000000000000000000, 1.000000000000000000, 1.000000000000000000, 1.000000000000000000, 1.000000000000000000, 1.000000000000000000, 1.000000000000000000, 1.000000000000000000, 1.000000000000000000, 1.000000000000000000, 1.000000000000000000, 1.000000000000000000, 1.000000000000000000, 1.000000000000000000, 1.000000000000000000),
 ( 0.3333333333333329818, 0.3333333333333329818, 0.3333333333333329818, 0.3333333333333329818, 0.3333333333333329818, 0.3333333333333329818, 0.3333333333333329818, 0.3333333333333329818, 0.3333333333333329818, 0.3333333333333329818, 0.3333333333333329818, 0.3333333333333329818, 0.3333333333333329818, 0.3333333333333329818, 0.3333333333333329818, 0.3333333333333329818, 0.3333333333333329818, 0.3333333333333329818, 0.3333333333333329818, 0.3333333333333329818, 0.3333333333333329818, 0.3333333333333329818, 0.3333333333333329818, 0.3333333333333329818, 0.3333333333333329818, 0.3333333333333329818, 0.3333333333333329818, 0.3333333333333329818, 0.3333333333333329818, 0.3333333333333329818, 0.3333333333333329818, 0.3333333333333329818, 0.3333333333333329818, 0.3333333333333329818, 0.3333333333333329818, 0.3333333333333329818, 0.3333333333333329818, 0.3333333333333329818, 0.3333333333333329818, 0.3333333333333329818, 0.3333333333333329818, 0.3333333333333329818, 0.3333333333333329818, 0.3333333333333329818, 0.3333333333333329818, 0.3333333333333329818, 0.3333333333333329818, 0.3333333333333329818, 0.3333333333333329818, 0.3333333333333329818, 0.3333333333333329818, 0.3333333333333329818, 0.3333333333333329818, 0.3333333333333329818, 0.3333333333333329818, 0.3333333333333329818, 0.3333333333333329818, 0.3333333333333329818, 0.3333333333333329818, 0.3333333333333329818, 0.3333333333333329818, 0.3333333333333329818, 0.3333333333333329818, 0.3333333333333329818, 0.3333333333333329818, 0.3333333333333329818, 0.3333333333333329818, 0.3333333333333329818, 0.3333333333333329818, 0.3333333333333329818, 0.3333333333333329818, 0.3333333333333329818, 0.3333333333333329818, 0.3333333333333329818, 0.3333333333333329818, 0.3333333333333329818, 0.3333333333333329818, 0.3333333333333329818, 0.3333333333333329818, 0.3333333333333329818, 0.3333333333333329818, 0.3333333333333329818, 0.3333333333333329818, 0.3333333333333329818, 0.3333333333333329818, 0.3333333333333329818, 0.3333333333333329818, 0.3333333333333329818, 0.3333333333333329818, 0.3333333333333329818, 0.3333333333333329818, 0.3333333333333329818, 0.3333333333333329818, 0.3333333333333329818, 0.3333333333333329818, 0.3333333333333329818, 0.3333333333333329818, 0.3333333333333329818, 0.3333333333333329818, 0.3333333333333329818, 0.3333333333333329818, 0.3333333333333329818, 0.3333333333333329818, 0.3333333333333329818, 0.3333333333333329818, 0.3333333333333329818, 0.3333333333333329818, 0.3333333333333329818, 0.3333333333333329818, 0.3333333333333329818, 0.3333333333333329818, 0.3333333333333329818, 0.3333333333333329818, 0.3333333333333329818, 0.3333333333333329818, 0.3333333333333329818, 0.3333333333333329818, 0.3333333333333329818, 0.3333333333333329818, 0.3333333333333329818, 0.3333333333333329818, 0.3333333333333329818, 0.3333333333333329818, 0.3333333333333329818, 0.3333333333333329818, 0.3333333333333329818, 0.3333333333333329818, 0.3333333333333329818, 0.3333333333333329818, 0.3333333333333329818, 0.3333333333333329818, 0.3333333333333329818, 0.3333333333333329818, 0.3333333333333329818, 0.3333333333333329818, 0.3333333333333329818, 0.3333333333333329818, 0.3333333333333329818, 0.3333333333333329818, 0.3333333333333329818, 0.3333333333333329818, 0.3333333333333329818, 0.3333333333333329818, 0.3333333333333329818, 0.3333333333333329818, 0.3333333333333329818, 0.3333333333333329818, 0.3333333333333329818, 0.3333333333333329818, 0.3333333333333329818, 0.3333333333333329818, 0.3333333333333329818, 0.3333333333333329818, 0.3333333333333329818, 0.3333333333333329818, 0.3333333333333329818, 0.3333333333333329818, 0.3333333333333329818, 0.3333333333333329818, 0.3333333333333329818, 0.3333333333333329818, 0.3333333333333329818, 0.3333333333333329818, 0.3333333333333329818, 0.3333333333333329818, 0.3333333333333329818, 0.3333333333333329818, 0.3333333333333329818, 0.3333333333333329818, 0.3333333333333329818, 0.3333333333333329818, 0.3333333333333329818, 0.3333333333333329818, 0.3333333333333329818, 0.3333333333333329818, 0.3333333333333329818, 0.3333333333333329818, 0.3333333333333329818, 0.3333333333333329818, 0.3333333333333329818, 0.3333333333333329818, 0.3333333333333329818, 0.3333333333333329818, 0.3333333333333329818, 0.3333333333333329818, 0.3333333333333329818, 0.3333333333333329818, 0.3333333333333329818),
 ( 0.3333333333333329818, 0.3333333333333329818, 0.3333333333333329818, 0.3333333333333329818, 0.3333333333333329818, 0.3333333333333329818, 0.3333333333333329818, 0.3333333333333329818, 0.3333333333333329818, 0.3333333333333329818, 0.3333333333333329818, 0.3333333333333329818, 0.3333333333333329818, 0.3333333333333329818, 0.3333333333333329818, 0.3333333333333329818, 0.3333333333333329818, 0.3333333333333329818, 0.3333333333333329818, 0.3333333333333329818, 0.3333333333333329818, 0.3333333333333329818, 0.3333333333333329818, 0.3333333333333329818, 0.3333333333333329818, 0.3333333333333329818, 0.3333333333333329818, 0.3333333333333329818, 0.3333333333333329818, 0.3333333333333329818, 0.3333333333333329818, 0.3333333333333329818, 0.3333333333333329818, 0.3333333333333329818, 0.3333333333333329818, 0.3333333333333329818, 0.3333333333333329818, 0.3333333333333329818, 0.3333333333333329818, 0.3333333333333329818, 0.3333333333333329818, 0.3333333333333329818, 0.3333333333333329818, 0.3333333333333329818, 0.3333333333333329818, 0.3333333333333329818, 0.3333333333333329818, 0.3333333333333329818, 0.3333333333333329818, 0.3333333333333329818, 0.3333333333333329818, 0.3333333333333329818, 0.3333333333333329818, 0.3333333333333329818, 0.3333333333333329818, 0.3333333333333329818, 0.3333333333333329818, 0.3333333333333329818, 0.3333333333333329818, 0.3333333333333329818, 0.3333333333333329818, 0.3333333333333329818, 0.3333333333333329818, 0.3333333333333329818, 0.3333333333333329818, 0.3333333333333329818, 0.3333333333333329818, 0.3333333333333329818, 0.3333333333333329818, 0.3333333333333329818, 0.3333333333333329818, 0.3333333333333329818, 0.3333333333333329818, 0.3333333333333329818, 0.3333333333333329818, 0.3333333333333329818, 0.3333333333333329818, 0.3333333333333329818, 0.3333333333333329818, 0.3333333333333329818, 0.3333333333333329818, 0.3333333333333329818, 0.3333333333333329818, 0.3333333333333329818, 0.3333333333333329818, 0.3333333333333329818, 0.3333333333333329818, 0.3333333333333329818, 0.3333333333333329818, 0.3333333333333329818, 0.3333333333333329818, 0.3333333333333329818, 0.3333333333333329818, 0.3333333333333329818, 0.3333333333333329818, 0.3333333333333329818, 0.3333333333333329818, 0.3333333333333329818, 0.3333333333333329818, 0.3333333333333329818, 0.3333333333333329818, 0.3333333333333329818, 0.3333333333333329818, 0.3333333333333329818, 0.3333333333333329818, 0.3333333333333329818, 0.3333333333333329818, 0.3333333333333329818, 0.3333333333333329818, 0.3333333333333329818, 0.3333333333333329818, 0.3333333333333329818, 0.3333333333333329818, 0.3333333333333329818, 0.3333333333333329818, 0.3333333333333329818, 0.3333333333333329818, 0.3333333333333329818, 0.3333333333333329818, 0.3333333333333329818, 0.3333333333333329818, 0.3333333333333329818, 0.3333333333333329818, 0.3333333333333329818, 0.3333333333333329818, 0.3333333333333329818, 0.3333333333333329818, 0.3333333333333329818, 0.3333333333333329818, 0.3333333333333329818, 0.3333333333333329818, 0.3333333333333329818, 0.3333333333333329818, 0.3333333333333329818, 0.3333333333333329818, 0.3333333333333329818, 0.3333333333333329818, 0.3333333333333329818, 0.3333333333333329818, 0.3333333333333329818, 0.3333333333333329818, 0.3333333333333329818, 0.3333333333333329818, 0.3333333333333329818, 0.3333333333333329818, 0.3333333333333329818, 0.3333333333333329818, 0.3333333333333329818, 0.3333333333333329818, 0.3333333333333329818, 0.3333333333333329818, 0.3333333333333329818, 0.3333333333333329818, 0.3333333333333329818, 0.3333333333333329818, 0.3333333333333329818, 0.3333333333333329818, 0.3333333333333329818, 0.3333333333333329818, 0.3333333333333329818, 0.3333333333333329818, 0.3333333333333329818, 0.3333333333333329818, 0.3333333333333329818, 0.3333333333333329818, 0.3333333333333329818, 0.3333333333333329818, 0.3333333333333329818, 0.3333333333333329818, 0.3333333333333329818, 0.3333333333333329818, 0.3333333333333329818, 0.3333333333333329818, 0.3333333333333329818, 0.3333333333333329818, 0.3333333333333329818, 0.3333333333333329818, 0.3333333333333329818, 0.3333333333333329818, 0.3333333333333329818, 0.3333333333333329818, 0.3333333333333329818, 0.3333333333333329818, 0.3333333333333329818, 0.3333333333333329818, 0.3333333333333329818, 0.3333333333333329818, 0.3333333333333329818),
 ( 1.000000000000000000, 1.000000000000000000, 1.000000000000000000, 1.000000000000000000, 1.000000000000000000, 1.000000000000000000, 1.000000000000000000, 1.000000000000000000, 1.000000000000000000, 1.000000000000000000, 1.000000000000000000, 1.000000000000000000, 1.000000000000000000, 1.000000000000000000, 1.000000000000000000, 1.000000000000000000, 1.000000000000000000, 1.000000000000000000, 1.000000000000000000, 1.000000000000000000, 1.000000000000000000, 1.000000000000000000, 1.000000000000000000, 1.000000000000000000, 1.000000000000000000, 1.000000000000000000, 1.000000000000000000, 1.000000000000000000, 1.000000000000000000, 1.000000000000000000, 1.000000000000000000, 1.000000000000000000, 1.000000000000000000, 1.000000000000000000, 1.000000000000000000, 1.000000000000000000, 1.000000000000000000, 1.000000000000000000, 1.000000000000000000, 1.000000000000000000, 1.000000000000000000, 1.000000000000000000, 1.000000000000000000, 1.000000000000000000, 1.000000000000000000, 1.000000000000000000, 1.000000000000000000, 1.000000000000000000, 1.000000000000000000, 1.000000000000000000, 1.000000000000000000, 1.000000000000000000, 1.000000000000000000, 1.000000000000000000, 1.000000000000000000, 1.000000000000000000, 1.000000000000000000, 1.000000000000000000, 1.000000000000000000, 1.000000000000000000, 1.000000000000000000, 1.000000000000000000, 1.000000000000000000, 1.000000000000000000, 1.000000000000000000, 1.000000000000000000, 1.000000000000000000, 1.000000000000000000, 1.000000000000000000, 1.000000000000000000, 1.000000000000000000, 1.000000000000000000, 1.000000000000000000, 1.000000000000000000, 1.000000000000000000, 1.000000000000000000, 1.000000000000000000, 1.000000000000000000, 1.000000000000000000, 1.000000000000000000, 1.000000000000000000, 1.000000000000000000, 1.000000000000000000, 1.000000000000000000, 1.000000000000000000, 1.000000000000000000, 1.000000000000000000, 1.000000000000000000, 1.000000000000000000, 1.000000000000000000, 1.000000000000000000, 1.000000000000000000, 1.000000000000000000, 1.000000000000000000, 1.000000000000000000, 1.000000000000000000, 1.000000000000000000, 1.000000000000000000, 1.000000000000000000, 1.000000000000000000, 1.000000000000000000, 1.000000000000000000, 1.000000000000000000, 1.000000000000000000, 1.000000000000000000, 1.000000000000000000, 1.000000000000000000, 1.000000000000000000, 1.000000000000000000, 1.000000000000000000, 1.000000000000000000, 1.000000000000000000, 1.000000000000000000, 1.000000000000000000, 1.000000000000000000, 1.000000000000000000, 1.000000000000000000, 1.000000000000000000, 1.000000000000000000, 1.000000000000000000, 1.000000000000000000, 1.000000000000000000, 1.000000000000000000, 1.000000000000000000, 1.000000000000000000, 1.000000000000000000, 1.000000000000000000, 1.000000000000000000, 1.000000000000000000, 1.000000000000000000, 1.000000000000000000, 1.000000000000000000, 1.000000000000000000, 1.000000000000000000, 1.000000000000000000, 1.000000000000000000, 1.000000000000000000, 1.000000000000000000, 1.000000000000000000, 1.000000000000000000, 1.000000000000000000, 1.000000000000000000, 1.000000000000000000, 1.000000000000000000, 1.000000000000000000, 1.000000000000000000, 1.000000000000000000, 1.000000000000000000, 1.000000000000000000, 1.000000000000000000, 1.000000000000000000, 1.000000000000000000, 1.000000000000000000, 1.000000000000000000, 1.000000000000000000, 1.000000000000000000, 1.000000000000000000, 1.000000000000000000, 1.000000000000000000, 1.000000000000000000, 1.000000000000000000, 1.000000000000000000, 1.000000000000000000, 1.000000000000000000, 1.000000000000000000, 1.000000000000000000, 1.000000000000000000, 1.000000000000000000, 1.000000000000000000, 1.000000000000000000, 1.000000000000000000, 1.000000000000000000, 1.000000000000000000, 1.000000000000000000, 1.000000000000000000, 1.000000000000000000, 1.000000000000000000, 1.000000000000000000, 1.000000000000000000, 1.000000000000000000, 1.000000000000000000, 1.000000000000000000, 1.000000000000000000, 1.000000000000000000, 1.000000000000000000, 1.000000000000000000, 1.000000000000000000, 1.000000000000000000),
 ( 0.3333333333333329818, 0.3333333333333329818, 0.3333333333333329818, 0.3333333333333329818, 0.3333333333333329818, 0.3333333333333329818, 0.3333333333333329818, 0.3333333333333329818, 0.3333333333333329818, 0.3333333333333329818, 0.3333333333333329818, 0.3333333333333329818, 0.3333333333333329818, 0.3333333333333329818, 0.3333333333333329818, 0.3333333333333329818, 0.3333333333333329818, 0.3333333333333329818, 0.3333333333333329818, 0.3333333333333329818, 0.3333333333333329818, 0.3333333333333329818, 0.3333333333333329818, 0.3333333333333329818, 0.3333333333333329818, 0.3333333333333329818, 0.3333333333333329818, 0.3333333333333329818, 0.3333333333333329818, 0.3333333333333329818, 0.3333333333333329818, 0.3333333333333329818, 0.3333333333333329818, 0.3333333333333329818, 0.3333333333333329818, 0.3333333333333329818, 0.3333333333333329818, 0.3333333333333329818, 0.3333333333333329818, 0.3333333333333329818, 0.3333333333333329818, 0.3333333333333329818, 0.3333333333333329818, 0.3333333333333329818, 0.3333333333333329818, 0.3333333333333329818, 0.3333333333333329818, 0.3333333333333329818, 0.3333333333333329818, 0.3333333333333329818, 0.3333333333333329818, 0.3333333333333329818, 0.3333333333333329818, 0.3333333333333329818, 0.3333333333333329818, 0.3333333333333329818, 0.3333333333333329818, 0.3333333333333329818, 0.3333333333333329818, 0.3333333333333329818, 0.3333333333333329818, 0.3333333333333329818, 0.3333333333333329818, 0.3333333333333329818, 0.3333333333333329818, 0.3333333333333329818, 0.3333333333333329818, 0.3333333333333329818, 0.3333333333333329818, 0.3333333333333329818, 0.3333333333333329818, 0.3333333333333329818, 0.3333333333333329818, 0.3333333333333329818, 0.3333333333333329818, 0.3333333333333329818, 0.3333333333333329818, 0.3333333333333329818, 0.3333333333333329818, 0.3333333333333329818, 0.3333333333333329818, 0.3333333333333329818, 0.3333333333333329818, 0.3333333333333329818, 0.3333333333333329818, 0.3333333333333329818, 0.3333333333333329818, 0.3333333333333329818, 0.3333333333333329818, 0.3333333333333329818, 0.3333333333333329818, 0.3333333333333329818, 0.3333333333333329818, 0.3333333333333329818, 0.3333333333333329818, 0.3333333333333329818, 0.3333333333333329818, 0.3333333333333329818, 0.3333333333333329818, 0.3333333333333329818, 0.3333333333333329818, 0.3333333333333329818, 0.3333333333333329818, 0.3333333333333329818, 0.3333333333333329818, 0.3333333333333329818, 0.3333333333333329818, 0.3333333333333329818, 0.3333333333333329818, 0.3333333333333329818, 0.3333333333333329818, 0.3333333333333329818, 0.3333333333333329818, 0.3333333333333329818, 0.3333333333333329818, 0.3333333333333329818, 0.3333333333333329818, 0.3333333333333329818, 0.3333333333333329818, 0.3333333333333329818, 0.3333333333333329818, 0.3333333333333329818, 0.3333333333333329818, 0.3333333333333329818, 0.3333333333333329818, 0.3333333333333329818, 0.3333333333333329818, 0.3333333333333329818, 0.3333333333333329818, 0.3333333333333329818, 0.3333333333333329818, 0.3333333333333329818, 0.3333333333333329818, 0.3333333333333329818, 0.3333333333333329818, 0.3333333333333329818, 0.3333333333333329818, 0.3333333333333329818, 0.3333333333333329818, 0.3333333333333329818, 0.3333333333333329818, 0.3333333333333329818, 0.3333333333333329818, 0.3333333333333329818, 0.3333333333333329818, 0.3333333333333329818, 0.3333333333333329818, 0.3333333333333329818, 0.3333333333333329818, 0.3333333333333329818, 0.3333333333333329818, 0.3333333333333329818, 0.3333333333333329818, 0.3333333333333329818, 0.3333333333333329818, 0.3333333333333329818, 0.3333333333333329818, 0.3333333333333329818, 0.3333333333333329818, 0.3333333333333329818, 0.3333333333333329818, 0.3333333333333329818, 0.3333333333333329818, 0.3333333333333329818, 0.3333333333333329818, 0.3333333333333329818, 0.3333333333333329818, 0.3333333333333329818, 0.3333333333333329818, 0.3333333333333329818, 0.3333333333333329818, 0.3333333333333329818, 0.3333333333333329818, 0.3333333333333329818, 0.3333333333333329818, 0.3333333333333329818, 0.3333333333333329818, 0.3333333333333329818, 0.3333333333333329818, 0.3333333333333329818, 0.3333333333333329818, 0.3333333333333329818, 0.3333333333333329818, 0.3333333333333329818, 0.3333333333333329818, 0.3333333333333329818, 0.3333333333333329818, 0.3333333333333329818),
 ( 0.3333333333333329818, 0.3333333333333329818, 0.3333333333333329818, 0.3333333333333329818, 0.3333333333333329818, 0.3333333333333329818, 0.3333333333333329818, 0.3333333333333329818, 0.3333333333333329818, 0.3333333333333329818, 0.3333333333333329818, 0.3333333333333329818, 0.3333333333333329818, 0.3333333333333329818, 0.3333333333333329818, 0.3333333333333329818, 0.3333333333333329818, 0.3333333333333329818, 0.3333333333333329818, 0.3333333333333329818, 0.3333333333333329818, 0.3333333333333329818, 0.3333333333333329818, 0.3333333333333329818, 0.3333333333333329818, 0.3333333333333329818, 0.3333333333333329818, 0.3333333333333329818, 0.3333333333333329818, 0.3333333333333329818, 0.3333333333333329818, 0.3333333333333329818, 0.3333333333333329818, 0.3333333333333329818, 0.3333333333333329818, 0.3333333333333329818, 0.3333333333333329818, 0.3333333333333329818, 0.3333333333333329818, 0.3333333333333329818, 0.3333333333333329818, 0.3333333333333329818, 0.3333333333333329818, 0.3333333333333329818, 0.3333333333333329818, 0.3333333333333329818, 0.3333333333333329818, 0.3333333333333329818, 0.3333333333333329818, 0.3333333333333329818, 0.3333333333333329818, 0.3333333333333329818, 0.3333333333333329818, 0.3333333333333329818, 0.3333333333333329818, 0.3333333333333329818, 0.3333333333333329818, 0.3333333333333329818, 0.3333333333333329818, 0.3333333333333329818, 0.3333333333333329818, 0.3333333333333329818, 0.3333333333333329818, 0.3333333333333329818, 0.3333333333333329818, 0.3333333333333329818, 0.3333333333333329818, 0.3333333333333329818, 0.3333333333333329818, 0.3333333333333329818, 0.3333333333333329818, 0.3333333333333329818, 0.3333333333333329818, 0.3333333333333329818, 0.3333333333333329818, 0.3333333333333329818, 0.3333333333333329818, 0.3333333333333329818, 0.3333333333333329818, 0.3333333333333329818, 0.3333333333333329818, 0.3333333333333329818, 0.3333333333333329818, 0.3333333333333329818, 0.3333333333333329818, 0.3333333333333329818, 0.3333333333333329818, 0.3333333333333329818, 0.3333333333333329818, 0.3333333333333329818, 0.3333333333333329818, 0.3333333333333329818, 0.3333333333333329818, 0.3333333333333329818, 0.3333333333333329818, 0.3333333333333329818, 0.3333333333333329818, 0.3333333333333329818, 0.3333333333333329818, 0.3333333333333329818, 0.3333333333333329818, 0.3333333333333329818, 0.3333333333333329818, 0.3333333333333329818, 0.3333333333333329818, 0.3333333333333329818, 0.3333333333333329818, 0.3333333333333329818, 0.3333333333333329818, 0.3333333333333329818, 0.3333333333333329818, 0.3333333333333329818, 0.3333333333333329818, 0.3333333333333329818, 0.3333333333333329818, 0.3333333333333329818, 0.3333333333333329818, 0.3333333333333329818, 0.3333333333333329818, 0.3333333333333329818, 0.3333333333333329818, 0.3333333333333329818, 0.3333333333333329818, 0.3333333333333329818, 0.3333333333333329818, 0.3333333333333329818, 0.3333333333333329818, 0.3333333333333329818, 0.3333333333333329818, 0.3333333333333329818, 0.3333333333333329818, 0.3333333333333329818, 0.3333333333333329818, 0.3333333333333329818, 0.3333333333333329818, 0.3333333333333329818, 0.3333333333333329818, 0.3333333333333329818, 0.3333333333333329818, 0.3333333333333329818, 0.3333333333333329818, 0.3333333333333329818, 0.3333333333333329818, 0.3333333333333329818, 0.3333333333333329818, 0.3333333333333329818, 0.3333333333333329818, 0.3333333333333329818, 0.3333333333333329818, 0.3333333333333329818, 0.3333333333333329818, 0.3333333333333329818, 0.3333333333333329818, 0.3333333333333329818, 0.3333333333333329818, 0.3333333333333329818, 0.3333333333333329818, 0.3333333333333329818, 0.3333333333333329818, 0.3333333333333329818, 0.3333333333333329818, 0.3333333333333329818, 0.3333333333333329818, 0.3333333333333329818, 0.3333333333333329818, 0.3333333333333329818, 0.3333333333333329818, 0.3333333333333329818, 0.3333333333333329818, 0.3333333333333329818, 0.3333333333333329818, 0.3333333333333329818, 0.3333333333333329818, 0.3333333333333329818, 0.3333333333333329818, 0.3333333333333329818, 0.3333333333333329818, 0.3333333333333329818, 0.3333333333333329818, 0.3333333333333329818, 0.3333333333333329818, 0.3333333333333329818, 0.3333333333333329818, 0.3333333333333329818, 0.3333333333333329818, 0.3333333333333329818, 0.3333333333333329818, 0.3333333333333329818),
 ( 1.000000000000000000, 1.000000000000000000, 1.000000000000000000, 1.000000000000000000, 1.000000000000000000, 1.000000000000000000, 1.000000000000000000, 1.000000000000000000, 1.000000000000000000, 1.000000000000000000, 1.000000000000000000, 1.000000000000000000, 1.000000000000000000, 1.000000000000000000, 1.000000000000000000, 1.000000000000000000, 1.000000000000000000, 1.000000000000000000, 1.000000000000000000, 1.000000000000000000, 1.000000000000000000, 1.000000000000000000, 1.000000000000000000, 1.000000000000000000, 1.000000000000000000, 1.000000000000000000, 1.000000000000000000, 1.000000000000000000, 1.000000000000000000, 1.000000000000000000, 1.000000000000000000, 1.000000000000000000, 1.000000000000000000, 1.000000000000000000, 1.000000000000000000, 1.000000000000000000, 1.000000000000000000, 1.000000000000000000, 1.000000000000000000, 1.000000000000000000, 1.000000000000000000, 1.000000000000000000, 1.000000000000000000, 1.000000000000000000, 1.000000000000000000, 1.000000000000000000, 1.000000000000000000, 1.000000000000000000, 1.000000000000000000, 1.000000000000000000, 1.000000000000000000, 1.000000000000000000, 1.000000000000000000, 1.000000000000000000, 1.000000000000000000, 1.000000000000000000, 1.000000000000000000, 1.000000000000000000, 1.000000000000000000, 1.000000000000000000, 1.000000000000000000, 1.000000000000000000, 1.000000000000000000, 1.000000000000000000, 1.000000000000000000, 1.000000000000000000, 1.000000000000000000, 1.000000000000000000, 1.000000000000000000, 1.000000000000000000, 1.000000000000000000, 1.000000000000000000, 1.000000000000000000, 1.000000000000000000, 1.000000000000000000, 1.000000000000000000, 1.000000000000000000, 1.000000000000000000, 1.000000000000000000, 1.000000000000000000, 1.000000000000000000, 1.000000000000000000, 1.000000000000000000, 1.000000000000000000, 1.000000000000000000, 1.000000000000000000, 1.000000000000000000, 1.000000000000000000, 1.000000000000000000, 1.000000000000000000, 1.000000000000000000, 1.000000000000000000, 1.000000000000000000, 1.000000000000000000, 1.000000000000000000, 1.000000000000000000, 1.000000000000000000, 1.000000000000000000, 1.000000000000000000, 1.000000000000000000, 1.000000000000000000, 1.000000000000000000, 1.000000000000000000, 1.000000000000000000, 1.000000000000000000, 1.000000000000000000, 1.000000000000000000, 1.000000000000000000, 1.000000000000000000, 1.000000000000000000, 1.000000000000000000, 1.000000000000000000, 1.000000000000000000, 1.000000000000000000, 1.000000000000000000, 1.000000000000000000, 1.000000000000000000, 1.000000000000000000, 1.000000000000000000, 1.000000000000000000, 1.000000000000000000, 1.000000000000000000, 1.000000000000000000, 1.000000000000000000, 1.000000000000000000, 1.000000000000000000, 1.000000000000000000, 1.000000000000000000, 1.000000000000000000, 1.000000000000000000, 1.000000000000000000, 1.000000000000000000, 1.000000000000000000, 1.000000000000000000, 1.000000000000000000, 1.000000000000000000, 1.000000000000000000, 1.000000000000000000, 1.000000000000000000, 1.000000000000000000, 1.000000000000000000, 1.000000000000000000, 1.000000000000000000, 1.000000000000000000, 1.000000000000000000, 1.000000000000000000, 1.000000000000000000, 1.000000000000000000, 1.000000000000000000, 1.000000000000000000, 1.000000000000000000, 1.000000000000000000, 1.000000000000000000, 1.000000000000000000, 1.000000000000000000, 1.000000000000000000, 1.000000000000000000, 1.000000000000000000, 1.000000000000000000, 1.000000000000000000, 1.000000000000000000, 1.000000000000000000, 1.000000000000000000, 1.000000000000000000, 1.000000000000000000, 1.000000000000000000, 1.000000000000000000, 1.000000000000000000, 1.000000000000000000, 1.000000000000000000, 1.000000000000000000, 1.000000000000000000, 1.000000000000000000, 1.000000000000000000, 1.000000000000000000, 1.000000000000000000, 1.000000000000000000, 1.000000000000000000, 1.000000000000000000, 1.000000000000000000, 1.000000000000000000, 1.000000000000000000, 1.000000000000000000, 1.000000000000000000, 1.000000000000000000, 1.000000000000000000, 1.000000000000000000, 1.000000000000000000) ) ) 
 REPRESENTATION_ITEM ( '' )  SURFACE ( )  );
#3229 = CARTESIAN_POINT ( 'NONE',  ( -2.239137794397029868, -4.987178660919110662, 3.975425900939220103 ) ) ;
#3230 = VECTOR ( 'NONE', #8812, 1000.000000000000000 ) ;
#3231 = FACE_BOUND ( 'NONE', #12525, .T. ) ;
#3232 = CARTESIAN_POINT ( 'NONE',  ( 1.912899118714319169, -4.218665147405596727, 5.445465495009710111 ) ) ;
#3233 = DIRECTION ( 'NONE',  ( -0.7071067811865480168, 0.000000000000000000, 0.7071067811865470176 ) ) ;
#3234 = ORIENTED_EDGE ( 'NONE', *, *, #12205, .T. ) ;
#3235 = VERTEX_POINT ( 'NONE', #2857 ) ;
#3236 = CARTESIAN_POINT ( 'NONE',  ( 1.899999999999999911, 2.481229107598850043E-16, 3.278889744907200310 ) ) ;
#3237 = ORIENTED_EDGE ( 'NONE', *, *, #9596, .F. ) ;
#3238 = EDGE_CURVE ( 'NONE', #16266, #4541, #14191, .T. ) ;
#3239 = PLANE ( 'NONE',  #5548 ) ;
#3240 = DIRECTION ( 'NONE',  ( 5.551115123125780730E-16, 0.000000000000000000, 1.000000000000000000 ) ) ;
#3241 = ORIENTED_EDGE ( 'NONE', *, *, #12998, .F. ) ;
#3242 = CARTESIAN_POINT ( 'NONE',  ( 1.880631435828169939, -5.355296610169490101, 3.876649216148224220 ) ) ;
#3243 = PLANE ( 'NONE',  #9317 ) ;
#3244 = CARTESIAN_POINT ( 'NONE',  ( 1.713314936023349944, -5.338983050847460277, 3.089913064446569546 ) ) ;
#3245 = DIRECTION ( 'NONE',  ( 1.000000000000000000, 0.000000000000000000, 0.000000000000000000 ) ) ;
#3246 = FACE_OUTER_BOUND ( 'NONE', #9018, .T. ) ;
#3247 = CARTESIAN_POINT ( 'NONE',  ( 1.000000000000000000, -5.599999999999999645, 5.100000000000000533 ) ) ;
#3248 = ADVANCED_FACE ( 'NONE', ( #2990 ), #5581, .F. ) ;
#3249 = CARTESIAN_POINT ( 'NONE',  ( -2.349129089426440054, -4.894025507765950245, 4.842612091679129982 ) ) ;
#3250 = CARTESIAN_POINT ( 'NONE',  ( -1.876226141297921091, -4.711560077819614278, 3.866526959224360294 ) ) ;
#3251 = ADVANCED_FACE ( 'NONE', ( #15491 ), #8444, .T. ) ;
#3252 = CARTESIAN_POINT ( 'NONE',  ( -0.009340024727882490982, -5.298031483068750269, 2.378874508206550331 ) ) ;
#3253 = CIRCLE ( 'NONE', #7121, 0.5999999999999998668 ) ;
#3254 = LINE ( 'NONE', #13070, #9449 ) ;
#3255 = EDGE_LOOP ( 'NONE', ( #11108, #6254, #9730, #5011 ) ) ;
#3256 = ADVANCED_FACE ( 'NONE', ( #11495 ), #12713, .T. ) ;
#3257 = CARTESIAN_POINT ( 'NONE',  ( 0.8731223871105069367, -0.1290254237288140371, 6.558046933601105799 ) ) ;
#3258 = CARTESIAN_POINT ( 'NONE',  ( -1.097561405233230092, -3.613169651910099756, 2.618148744692269769 ) ) ;
#3259 = EDGE_LOOP ( 'NONE', ( #7078, #14668, #11387 ) ) ;
#3260 = EDGE_CURVE ( 'NONE', #6043, #8260, #4262, .T. ) ;
#3261 = ORIENTED_EDGE ( 'NONE', *, *, #12184, .F. ) ;
#3262 = ADVANCED_FACE ( 'NONE', ( #200 ), #5844, .T. ) ;
#3263 = LINE ( 'NONE', #8905, #10014 ) ;
#3264 = ORIENTED_EDGE ( 'NONE', *, *, #9028, .F. ) ;
#3265 = CARTESIAN_POINT ( 'NONE',  ( -1.928817277882839409, -4.455388906648448888, 6.048484184565968924 ) ) ;
#3266 = DIRECTION ( 'NONE',  ( 0.000000000000000000, 0.000000000000000000, 1.000000000000000000 ) ) ;
#3267 = CARTESIAN_POINT ( 'NONE',  ( 1.932035991685901122, -5.038983050847454237, 2.884370051397200818 ) ) ;
#3268 = B_SPLINE_CURVE_WITH_KNOTS ( 'NONE', 3,
 ( #16327, #15140, #8099, #2451, #2167, #13738, #16417, #7906, #3442, #14751, #13557, #6695, #1056, #14945, #17695, #5123, #872, #2065, #12353, #3632, #7720, #2256, #13364, #9283, #3724, #6403, #13455, #15053, #772, #3832, #6316, #11978, #17590, #4925, #10582, #6510, #12074, #12169, #2359, #8007, #13652, #963, #6601, #12258, #17876, #5214, #16521, #18245, #11333, #5687, #7083, #2635, #9759, #8377, #4280, #2911, #5321, #15326, #9570, #15597, #6797, #8182, #15510, #8457, #4191, #12445, #16969, #14204, #2816, #16695, #9937, #1425, #1325, #15228, #11045, #8284, #12530, #14094, #12726, #2730, #15423, #9852, #43, #5596, #13925, #14010, #16612, #7175, #6972, #18063, #3913, #2532, #1242, #9656, #5405, #11240, #13831, #16884, #1150, #4002, #11134, #17977, #6885, #18143, #8558, #10967, #5491, #16789, #4104, #12621, #1524, #11683, #5951, #10382, #17140, #13162, #7256, #12991, #4464, #13078, #311, #12814, #11418, #15860, #14635, #16044, #4542, #7349, #7437, #3168, #10036, #17411, #11590, #126, #10121, #8824, #397, #10195, #8907, #3003, #5863, #11510, #11787, #1950, #5776, #17052, #12899, #15693, #14475, #4374, #17220, #17309, #15775, #8644, #14291, #4637, #1612, #3083, #8726, #1793, #14370, #6125, #479, #1869, #1697, #6037, #10296, #4731, #3343, #221, #15964, #3265, #8988, #14555, #7518, #16403, #10560, #661, #17572, #9463, #14929, #10756, #6300, #13638, #15028, #9268, #17496, #11958 ),
 .UNSPECIFIED., .F., .F.,
 ( 4, 1, 1, 1, 1, 1, 1, 1, 1, 1, 1, 1, 1, 1, 1, 1, 1, 1, 1, 1, 1, 1, 1, 1, 1, 1, 1, 1, 1, 1, 1, 1, 1, 1, 1, 1, 1, 1, 1, 1, 1, 1, 1, 1, 1, 1, 1, 1, 1, 1, 1, 1, 1, 1, 1, 1, 1, 1, 1, 1, 1, 1, 1, 1, 1, 1, 1, 1, 1, 1, 1, 1, 1, 1, 1, 1, 1, 1, 1, 1, 1, 1, 1, 1, 1, 1, 1, 1, 1, 1, 1, 1, 1, 1, 1, 1, 1, 1, 1, 1, 1, 1, 1, 1, 1, 1, 1, 1, 1, 1, 1, 1, 1, 1, 1, 1, 1, 1, 1, 1, 1, 1, 1, 1, 1, 1, 1, 1, 1, 1, 1, 1, 1, 1, 1, 1, 1, 1, 1, 1, 1, 1, 1, 1, 1, 1, 1, 1, 1, 1, 1, 1, 1, 1, 1, 1, 1, 1, 1, 1, 1, 1, 1, 1, 1, 1, 1, 1, 1, 1, 1, 1, 1, 1, 1, 1, 1, 1, 1, 1, 1, 1, 1, 1, 1, 4 ),
 ( 0.7853981633974479459, 0.8787968639095770085, 0.9721955644217059600, 1.065594264933839908, 1.158992965445959866, 1.252391665958090039, 1.345790366470219990, 1.439189066982349940, 1.532587767494480113, 1.625986468006610064, 1.719385168518740015, 1.812783869030869965, 1.906182569543000138, 1.999581270055129867, 2.092979970567249826, 2.186378671079379998, 2.279777371591510171, 2.373176072103639900, 2.466574772615769628, 2.559973473127900245, 2.653372173640029974, 2.746770874152160147, 2.840169574664289875, 2.933568275176409834, 3.026966975688540007, 3.120365676200670180, 3.213764376712799908, 3.307163077224930081, 3.400561777737059810, 3.493960478249190427, 3.587359178761320155, 3.680757879273439670, 3.774156579785570287, 3.867555280297700016, 3.960953980809830188, 4.054352681321960361, 4.147751381834090090, 4.241150082346219818, 4.334548782858350435, 4.427947483370480164, 4.521346183882600123, 4.614744884394729851, 4.708143584906859580, 4.801542285418989309, 4.894940985931119926, 4.988339686443250542, 5.081738386955380271, 5.175137087467510000, 5.268535787979639728, 5.361934488491760575, 5.455333189003890304, 5.548731889516020033, 5.642130590028149761, 5.735529290540279490, 5.828927991052410107, 5.922326691564539836, 6.015725392076670452, 6.109124092588789523, 6.202522793100920140, 6.295921493613049869, 6.389320194125180485, 6.482718894637310214, 6.576117595149439943, 6.669516295661569671, 6.762914996173699400, 6.856313696685830017, 6.949712397197949976, 7.043111097710079704, 7.136509798222209433, 7.229908498734340050, 7.323307199246470667, 7.416705899758600395, 7.510104600270730124, 7.603503300782859853, 7.696902001294989581, 7.790300701807110428, 7.883699402319240157, 7.977098102831369886, 8.070496803343500503, 8.163895503855631119, 8.257294204367759960, 8.350692904879890577, 8.444091605392019417, 8.537490305904137600, 8.630889006416269993, 8.724287706928398833, 8.817686407440529450, 8.911085107952660067, 9.004483808464788908, 9.097882508976921301, 9.191281209489050141, 9.284679910001178982, 9.378078610513298941, 9.471477311025429557, 9.564876011537560174, 9.658274712049690791, 9.751673412561819632, 9.845072113073950248, 9.938470813586080865, 10.03186951409819905, 10.12526821461029947, 10.21866691512249936, 10.31206561563459978, 10.40546431614669842, 10.49886301665890009, 10.59226171717100051, 10.68566041768310093, 10.77905911819519957, 10.87245781870739947, 10.96585651921949989, 11.05925521973160031, 11.15265392024380020, 11.24605262075590062, 11.33945132126800104, 11.43285002178009968, 11.52624872229229958, 11.61964742280439999, 11.71304612331650041, 11.80644482382869853, 11.89984352434079895, 11.99324222485290115, 12.08664092536500156, 12.18003962587719968, 12.27343832638930010, 12.36683702690140052, 12.46023572741360042, 12.55363442792569906, 12.64703312843779948, 12.74043182894989990, 12.83383052946209979, 12.92722922997419843, 13.02062793048630063, 13.11402663099850052, 13.20742533151059916, 13.30082403202269958, 13.39422273253480000, 13.48762143304700167, 13.58102013355910032, 13.67441883407120073, 13.76781753458340063, 13.86121623509549927, 13.95461493560759969, 14.04801363611970011, 14.14141233663190000, 14.23481103714399865, 14.32820973765609907, 14.42160843816829896, 14.51500713868040116, 14.60840583919249980, 14.70180453970460022, 14.79520324021680011, 14.88860194072889875, 14.98200064124100095, 15.07539934175320084, 15.16879804226530126, 15.26219674277739990, 15.35559544328959980, 15.44899414380170022, 15.54239284431380064, 15.63579154482589928, 15.72919024533809740, 15.82258894585020137, 15.91598764636230001, 16.00938634687449991, 16.10278504738660033, 16.19618374789870074, 16.28958244841080116, 16.38298114892299751, 16.47637984943510148, 16.56977854994720545, 16.66317725045940179, 16.75657595097149866, 16.84997465148359908, 16.94337335199570305, 17.03677205250789939, 17.13017075301999981, 17.22356945353210023, 17.31696815404430012, 17.41036685455640054, 17.50376555506850096, 17.59716425558059782, 17.69056295609280127, 17.78396165660489814, 17.87736035711699856, 17.97075905762920200, 18.06415775814129887 ),
 .UNSPECIFIED. ) ;
#3269 = DIRECTION ( 'NONE',  ( 1.000000000000000000, 0.000000000000000000, 0.000000000000000000 ) ) ;
#3270 = VECTOR ( 'NONE', #15729, 1000.000000000000000 ) ;
#3271 = CARTESIAN_POINT ( 'NONE',  ( -2.224278379903029901, -0.5091101694915259879, 5.468825643806110470 ) ) ;
#3272 = VERTEX_POINT ( 'NONE', #1775 ) ;
#3273 = ADVANCED_FACE ( 'NONE', ( #562 ), #10450, .T. ) ;
#3274 = FACE_OUTER_BOUND ( 'NONE', #17645, .T. ) ;
#3275 = CARTESIAN_POINT ( 'NONE',  ( -4.898587196589400133E-17, 5.318248954186070243, 6.599999999999999645 ) ) ;
#3276 = CARTESIAN_POINT ( 'NONE',  ( -1.772995665808888788, -4.777584066324515710, 5.735078843205186239 ) ) ;
#3277 = LINE ( 'NONE', #17421, #15616 ) ;
#3278 = CARTESIAN_POINT ( 'NONE',  ( -2.519547246525518425, -0.5402542372881364852, 3.866491354109200529 ) ) ;
#3279 = ORIENTED_EDGE ( 'NONE', *, *, #436, .F. ) ;
#3280 = LINE ( 'NONE', #1713, #13811 ) ;
#3281 = EDGE_CURVE ( 'NONE', #6472, #17115, #15846, .T. ) ;
#3282 = EDGE_LOOP ( 'NONE', ( #16106, #17648, #5702, #12208 ) ) ;
#3283 = VECTOR ( 'NONE', #12379, 1000.000000000000000 ) ;
#3284 = CARTESIAN_POINT ( 'NONE',  ( -0.008236272907982289393, -0.5805379513491200072, 2.272810616177410203 ) ) ;
#3285 = CARTESIAN_POINT ( 'NONE',  ( -1.851073041990159984, -5.493220338983049622, 6.153284478378270528 ) ) ;
#3286 = CARTESIAN_POINT ( 'NONE',  ( -1.477796163681079689, -0.1824152542372890207, 6.531563725478148896 ) ) ;
#3287 = CARTESIAN_POINT ( 'NONE',  ( -2.632194480419669080, -3.310421904162345719, 5.038623552414950524 ) ) ;
#3288 = EDGE_LOOP ( 'NONE', ( #16286, #14113, #9305, #1422 ) ) ;
#3289 = CARTESIAN_POINT ( 'NONE',  ( -1.832842064134660109, -2.871785303044850135, 6.176291182464519913 ) ) ;
#3290 = CARTESIAN_POINT ( 'NONE',  ( -2.500000000000000000, 9.199999999999999289, 0.5999999999999999778 ) ) ;
#3291 = CARTESIAN_POINT ( 'NONE',  ( -1.899999999999999911, 9.199999999999999289, 0.6099999999999999867 ) ) ;
#3292 = CARTESIAN_POINT ( 'NONE',  ( 1.160665242129880426, -2.499172690432241772, 6.393445611272976947 ) ) ;
#3293 = FACE_OUTER_BOUND ( 'NONE', #9550, .T. ) ;
#3294 = CARTESIAN_POINT ( 'NONE',  ( 1.149999999999999911, 9.299999999999998934, 7.500000000000000000 ) ) ;
#3295 = ORIENTED_EDGE ( 'NONE', *, *, #8241, .F. ) ;
#3296 = LINE ( 'NONE', #1383, #11459 ) ;
#3297 = EDGE_CURVE ( 'NONE', #13591, #17265, #2131, .T. ) ;
#3298 = CARTESIAN_POINT ( 'NONE',  ( 1.250000000000000000, 6.144112549695430303, 6.100000000000000533 ) ) ;
#3299 = CARTESIAN_POINT ( 'NONE',  ( -2.653886076156968699, -1.474488005747551567, 4.698454755023434792 ) ) ;
#3300 = ORIENTED_EDGE ( 'NONE', *, *, #9251, .F. ) ;
#3301 = CARTESIAN_POINT ( 'NONE',  ( -1.722199153441400066, -5.095857339597789526, 3.099360556065549943 ) ) ;
#3302 = FACE_OUTER_BOUND ( 'NONE', #17486, .T. ) ;
#3303 = CARTESIAN_POINT ( 'NONE',  ( 0.1749999999999999889, 5.200000000000000178, 1.600000000000000089 ) ) ;
#3304 = CARTESIAN_POINT ( 'NONE',  ( 1.713314936023349944, -5.038983050847460454, 3.089913064446569546 ) ) ;
#3305 = EDGE_LOOP ( 'NONE', ( #9084, #14268, #17891, #11631 ) ) ;
#3306 = ORIENTED_EDGE ( 'NONE', *, *, #14930, .T. ) ;
#3307 = CARTESIAN_POINT ( 'NONE',  ( -0.5999999999999999778, 7.347880794884128857E-17, 7.700000000000000178 ) ) ;
#3308 = CARTESIAN_POINT ( 'NONE',  ( 2.500000000000000000, -6.661338147750919275E-17, 9.955530934770520091 ) ) ;
#3309 = ORIENTED_EDGE ( 'NONE', *, *, #5048, .T. ) ;
#3310 = DIRECTION ( 'NONE',  ( -4.433365283261159518E-17, 1.000000000000000000, 0.000000000000000000 ) ) ;
#3311 = CARTESIAN_POINT ( 'NONE',  ( 1.818868030982612183, -2.355602084342530933, 2.767428454397789839 ) ) ;
#3312 =( REPRESENTATION_RELATIONSHIP ('NONE','NONE', #2757, #2027 ) REPRESENTATION_RELATIONSHIP_WITH_TRANSFORMATION ( #2240 )SHAPE_REPRESENTATION_RELATIONSHIP( ) );
#3313 = PLANE ( 'NONE',  #6424 ) ;
#3314 = CARTESIAN_POINT ( 'NONE',  ( 2.616666666666660035, 8.899094389694600942E-17, 4.000000000000000000 ) ) ;
#3315 = CARTESIAN_POINT ( 'NONE',  ( 1.669205944673859854, -2.452596113855660231, 6.359065158982410537 ) ) ;
#3316 = CARTESIAN_POINT ( 'NONE',  ( 1.112057765673850174, -5.020626044399135068, 2.286633591154370482 ) ) ;
#3317 = CARTESIAN_POINT ( 'NONE',  ( -2.479511223993290603, -1.866548030288480042, 3.753882785753710483 ) ) ;
#3318 = DIRECTION ( 'NONE',  ( 1.000000000000000000, 0.000000000000000000, 0.000000000000000000 ) ) ;
#3319 = CARTESIAN_POINT ( 'NONE',  ( -0.7778405029480311983, -4.614566048306495638, 6.599964735094220991 ) ) ;
#3320 = DIRECTION ( 'NONE',  ( 7.401486830834380223E-16, 1.769136588914770194E-30, -1.000000000000000000 ) ) ;
#3321 = ORIENTED_EDGE ( 'NONE', *, *, #1591, .F. ) ;
#3322 = CARTESIAN_POINT ( 'NONE',  ( -1.899999999999999911, 10.00000000000000000, 7.286648454926749993E-16 ) ) ;
#3323 = ORIENTED_EDGE ( 'NONE', *, *, #4848, .T. ) ;
#3324 = CARTESIAN_POINT ( 'NONE',  ( 1.875000000000000000, 12.00000000000000000, 8.300000000000000711 ) ) ;
#3325 = PLANE ( 'NONE',  #10300 ) ;
#3326 = ORIENTED_EDGE ( 'NONE', *, *, #8472, .F. ) ;
#3327 = CARTESIAN_POINT ( 'NONE',  ( 1.526791597786429922, -2.774791273531720392, 6.490992212270249695 ) ) ;
#3328 = CARTESIAN_POINT ( 'NONE',  ( 1.899999999999999911, 0.8000000000000000444, -1.333009822025779987E-15 ) ) ;
#3329 = CARTESIAN_POINT ( 'NONE',  ( 2.286166334984490067, -5.386440677966100488, 5.258525443163859947 ) ) ;
#3330 = DIRECTION ( 'NONE',  ( -1.762990951819940286E-17, -1.000000000000000000, -2.891205793294679017E-15 ) ) ;
#3331 = CARTESIAN_POINT ( 'NONE',  ( -0.3752419433106839453, -1.424070552810999812, 7.023346545710370314 ) ) ;
#3332 = CARTESIAN_POINT ( 'NONE',  ( 1.869848057046569867, -4.288530012270459935, 6.129130480762009725 ) ) ;
#3333 = CARTESIAN_POINT ( 'NONE',  ( -1.945780800405131350, -4.688271789531334832, 4.045142061754299689 ) ) ;
#3334 = DIRECTION ( 'NONE',  ( 6.123233995736769734E-17, 8.894960955186829541E-48, 1.000000000000000000 ) ) ;
#3335 = SPHERICAL_SURFACE ( 'NONE', #15082, 0.4166666666666670182 ) ;
#3336 = ORIENTED_EDGE ( 'NONE', *, *, #14331, .F. ) ;
#3337 = CARTESIAN_POINT ( 'NONE',  ( -1.940327948426050941, -0.2091101694915259990, 5.370677689277675526 ) ) ;
#3338 = CARTESIAN_POINT ( 'NONE',  ( 2.342931736853870017, -4.102223705964150646, 4.477701633099130163 ) ) ;
#3339 = VERTEX_POINT ( 'NONE', #17291 ) ;
#3340 = ORIENTED_EDGE ( 'NONE', *, *, #16621, .F. ) ;
#3341 = CARTESIAN_POINT ( 'NONE',  ( -0.5999999999999999778, 7.347880794884128857E-17, 7.599999999999999645 ) ) ;
#3342 = ORIENTED_EDGE ( 'NONE', *, *, #10583, .T. ) ;
#3343 = CARTESIAN_POINT ( 'NONE',  ( -1.480680413335759837, -4.385524041783591009, 6.529298007719828156 ) ) ;
#3344 = CARTESIAN_POINT ( 'NONE',  ( 0.3171869470818560743, -5.144279661016955885, 7.334814496515233095 ) ) ;
#3345 = FACE_OUTER_BOUND ( 'NONE', #17085, .T. ) ;
#3346 = DIRECTION ( 'NONE',  ( 2.261565420532729920E-16, 1.000000000000000000, 0.000000000000000000 ) ) ;
#3347 = ORIENTED_EDGE ( 'NONE', *, *, #3260, .T. ) ;
#3348 = ADVANCED_FACE ( 'NONE', ( #3246 ), #16594, .T. ) ;
#3349 = CARTESIAN_POINT ( 'NONE',  ( -0.1749999999999999889, 4.299999999999999822, 1.600000000000000089 ) ) ;
#3350 = PLANE ( 'NONE',  #1125 ) ;
#3351 = EDGE_CURVE ( 'NONE', #1059, #4743, #8944, .T. ) ;
#3352 = CARTESIAN_POINT ( 'NONE',  ( -1.992092870331710452, -3.403575057315514130, 4.203544726484199856 ) ) ;
#3353 = ADVANCED_FACE ( 'NONE', ( #431 ), #14589, .T. ) ;
#3354 = CARTESIAN_POINT ( 'NONE',  ( -2.020286629067959971, -0.4913135593220345210, 6.420841923842841581 ) ) ;
#3355 = ORIENTED_EDGE ( 'NONE', *, *, #1782, .F. ) ;
#3356 = EDGE_LOOP ( 'NONE', ( #5368, #10630, #16215, #17214 ) ) ;
#3357 = PLANE ( 'NONE',  #6453 ) ;
#3358 = CARTESIAN_POINT ( 'NONE',  ( 4.265698758777729940E-16, 2.350000000000000089, 7.700000000000000178 ) ) ;
#3359 = CARTESIAN_POINT ( 'NONE',  ( -0.2812789908084309398, -0.1557203389830509321, 7.036533610117277959 ) ) ;
#3360 = CARTESIAN_POINT ( 'NONE',  ( -1.837442528958838750, -3.543304787045241433, 2.785079989718828752 ) ) ;
#3361 = ORIENTED_EDGE ( 'NONE', *, *, #528, .T. ) ;
#3362 =( GEOMETRIC_REPRESENTATION_CONTEXT ( 3 ) GLOBAL_UNCERTAINTY_ASSIGNED_CONTEXT ( ( #8082 ) ) GLOBAL_UNIT_ASSIGNED_CONTEXT ( ( #4521, #11213, #15569 ) ) REPRESENTATION_CONTEXT ( 'NONE', 'WORKASPACE' ) );
#3363 = CARTESIAN_POINT ( 'NONE',  ( 0.09706517602699299418, -2.638902420161969520, 7.051451474958980725 ) ) ;
#3364 = EDGE_CURVE ( 'NONE', #4345, #14300, #14053, .T. ) ;
#3365 = CARTESIAN_POINT ( 'NONE',  ( -0.7500000000000000000, 6.450000000000000178, 3.200000000000000178 ) ) ;
#3366 = EDGE_CURVE ( 'NONE', #616, #1663, #3745, .T. ) ;
#3367 = CARTESIAN_POINT ( 'NONE',  ( 1.238036348455360258, -3.593722239981790523, 3.062267469172269330 ) ) ;
#3368 = LINE ( 'NONE', #8936, #15905 ) ;
#3369 = CARTESIAN_POINT ( 'NONE',  ( 0.9516466452860694591, -0.9621456634052125700, 6.519140045500582126 ) ) ;
#3370 = ORIENTED_EDGE ( 'NONE', *, *, #11676, .T. ) ;
#3371 = CARTESIAN_POINT ( 'NONE',  ( 0.5110358699406184479, -0.3612150962701983770, 2.697283651280069527 ) ) ;
#3372 = CARTESIAN_POINT ( 'NONE',  ( -2.642175029090489513, -1.497776294035840561, 4.450952196049505538 ) ) ;
#3373 = MECHANICAL_DESIGN_GEOMETRIC_PRESENTATION_REPRESENTATION (  '', ( #1035 ), #10472 ) ;
#3374 = ORIENTED_EDGE ( 'NONE', *, *, #17726, .F. ) ;
#3375 = CARTESIAN_POINT ( 'NONE',  ( -0.03714311608457869507, -4.521412895153340550, 7.053160869216429596 ) ) ;
#3376 = CARTESIAN_POINT ( 'NONE',  ( -1.899999999999999911, -2.607830583485270085E-17, -8.881784197001250351E-16 ) ) ;
#3377 = LINE ( 'NONE', #11721, #14787 ) ;
#3378 = CARTESIAN_POINT ( 'NONE',  ( -2.340070819011249803, -5.219915254237290192, 4.950151441910549899 ) ) ;
#3379 = ORIENTED_EDGE ( 'NONE', *, *, #13823, .T. ) ;
#3380 = EDGE_LOOP ( 'NONE', ( #13922, #7396, #3898, #1742 ) ) ;
#3381 = CARTESIAN_POINT ( 'NONE',  ( 0.5999999999999999778, 11.40000000000000036, 7.599999999999999645 ) ) ;
#3382 = DIRECTION ( 'NONE',  ( 0.9622640697945192834, -0.2721173643531200614, 0.000000000000000000 ) ) ;
#3383 = DIRECTION ( 'NONE',  ( 0.000000000000000000, -1.000000000000000000, 1.807003620809174385E-16 ) ) ;
#3384 = ORIENTED_EDGE ( 'NONE', *, *, #18169, .T. ) ;
#3385 = CARTESIAN_POINT ( 'NONE',  ( 2.494165244384159763, -2.472043525783979678, 3.793218093085234166 ) ) ;
#3386 = ADVANCED_FACE ( 'NONE', ( #12278 ), #696, .T. ) ;
#3387 = CARTESIAN_POINT ( 'NONE',  ( -1.875000000000000000, 12.00000000000000000, 8.300000000000000711 ) ) ;
#3388 = CARTESIAN_POINT ( 'NONE',  ( 1.250000000000000000, 0.5999999999999999778, 7.599999999999999645 ) ) ;
#3389 = CARTESIAN_POINT ( 'NONE',  ( -2.211317922628890376, -3.127956474216019966, 3.894507149290469705 ) ) ;
#3390 = CARTESIAN_POINT ( 'NONE',  ( -0.009452110982655099330, -5.299807955295455564, 2.649999999999998579 ) ) ;
#3391 = CARTESIAN_POINT ( 'NONE',  ( 1.256119432346080478, -1.261052534792989288, 7.037793332329536966 ) ) ;
#3392 = EDGE_CURVE ( 'NONE', #1178, #9534, #5573, .T. ) ;
#3393 = DIRECTION ( 'NONE',  ( 0.000000000000000000, 0.000000000000000000, -1.000000000000000000 ) ) ;
#3394 = CARTESIAN_POINT ( 'NONE',  ( 0.1565249325564390115, -0.4468220338983060480, 7.048192310558509810 ) ) ;
#3395 = DIRECTION ( 'NONE',  ( 0.000000000000000000, 0.000000000000000000, 1.000000000000000000 ) ) ;
#3396 = CARTESIAN_POINT ( 'NONE',  ( 2.586172839791708533, -5.364194915254235418, 4.104546363490930716 ) ) ;
#3397 = ORIENTED_EDGE ( 'NONE', *, *, #17367, .F. ) ;
#3398 = ORIENTED_EDGE ( 'NONE', *, *, #5352, .F. ) ;
#3399 = CARTESIAN_POINT ( 'NONE',  ( 1.899999999999999911, 4.700000000000000178, 1.600000000000000089 ) ) ;
#3400 = LINE ( 'NONE', #10644, #7069 ) ;
#3401 = EDGE_LOOP ( 'NONE', ( #10796, #3614, #10052, #3336 ) ) ;
#3402 = CARTESIAN_POINT ( 'NONE',  ( -0.1749999999999999889, 8.800000000000000711, -3.200000000000000178 ) ) ;
#3403 = CARTESIAN_POINT ( 'NONE',  ( 0.6673090596498160165, -2.239160642901090181, 2.443133963569570355 ) ) ;
#3404 = ADVANCED_FACE ( 'NONE', ( #8032 ), #11996, .T. ) ;
#3405 = CARTESIAN_POINT ( 'NONE',  ( 1.699999999999999956, 9.299999999999998934, 7.700000000000000178 ) ) ;
#3406 = CARTESIAN_POINT ( 'NONE',  ( -0.6207106781186559896, 6.450000000000000178, 2.628553390593269423 ) ) ;
#3407 = CARTESIAN_POINT ( 'NONE',  ( 1.889999999999999902, 4.700000000000000178, 0.6099999999999999867 ) ) ;
#3408 = CARTESIAN_POINT ( 'NONE',  ( 2.046174187462399985, -1.121322805063259986, 5.862719605943959245 ) ) ;
#3409 = CARTESIAN_POINT ( 'NONE',  ( -0.2564439965878500538, -4.544701183441629766, 7.039440566481220074 ) ) ;
#3410 = CARTESIAN_POINT ( 'NONE',  ( -0.9742769543504515850, -4.338947465207014353, 6.507120986223577042 ) ) ;
#3411 = AXIS2_PLACEMENT_3D ( 'NONE', #11384, #7047, #96 ) ;
#3412 = LINE ( 'NONE', #16393, #531 ) ;
#3413 = FACE_OUTER_BOUND ( 'NONE', #14009, .T. ) ;
#3414 = ORIENTED_EDGE ( 'NONE', *, *, #10999, .F. ) ;
#3415 = CARTESIAN_POINT ( 'NONE',  ( 0.1749999999999999889, 9.099999999999999645, 0.4000000000000000222 ) ) ;
#3416 = CARTESIAN_POINT ( 'NONE',  ( 1.921786527979010062, -0.05783898305084796132, 3.977907449687776431 ) ) ;
#3417 = CARTESIAN_POINT ( 'NONE',  ( -0.8986180677147959095, -3.636457940198390304, 2.524860635301629852 ) ) ;
#3418 = ORIENTED_EDGE ( 'NONE', *, *, #4617, .T. ) ;
#3419 = ORIENTED_EDGE ( 'NONE', *, *, #9432, .F. ) ;
#3420 = DIRECTION ( 'NONE',  ( 6.123233995736769734E-17, 8.894960955186829541E-48, 1.000000000000000000 ) ) ;
#3421 = ORIENTED_EDGE ( 'NONE', *, *, #14712, .F. ) ;
#3422 = CARTESIAN_POINT ( 'NONE',  ( 2.500000000000000000, 11.15000000000000036, -1.135674796306499891E-15 ) ) ;
#3423 = CARTESIAN_POINT ( 'NONE',  ( -1.973760952634090238, -5.259957627118655665, 2.925986839873730982 ) ) ;
#3424 = VECTOR ( 'NONE', #2460, 1000.000000000000000 ) ;
#3425 = CARTESIAN_POINT ( 'NONE',  ( -0.03000000000000110217, 11.40000000000000036, 7.649999999999999467 ) ) ;
#3426 = DIRECTION ( 'NONE',  ( 0.000000000000000000, 1.000000000000000000, -1.110223024625159992E-16 ) ) ;
#3427 = ORIENTED_EDGE ( 'NONE', *, *, #14242, .T. ) ;
#3428 = CARTESIAN_POINT ( 'NONE',  ( -0.5500000000000000444, 6.450000000000000178, 2.699264068711930253 ) ) ;
#3429 = CARTESIAN_POINT ( 'NONE',  ( 1.372465729645801602, -4.335106588847043696, 6.226839763556046847 ) ) ;
#3430 = AXIS2_PLACEMENT_3D ( 'NONE', #2557, #2288, #6825 ) ;
#3431 = EDGE_CURVE ( 'NONE', #8419, #1946, #4855, .T. ) ;
#3432 = CARTESIAN_POINT ( 'NONE',  ( 1.347262683220810553, -0.1245762711864410871, 6.986424775243341045 ) ) ;
#3433 = EDGE_LOOP ( 'NONE', ( #4165, #8700, #11689, #7623 ) ) ;
#3434 = VECTOR ( 'NONE', #16823, 1000.000000000000000 ) ;
#3435 = CARTESIAN_POINT ( 'NONE',  ( 2.386628511786341722, -0.05338983050847501133, 3.539457309197775459 ) ) ;
#3436 = AXIS2_PLACEMENT_3D ( 'NONE', #6869, #7238, #16951 ) ;
#3437 = ORIENTED_EDGE ( 'NONE', *, *, #6879, .T. ) ;
#3438 = DIRECTION ( 'NONE',  ( -1.556829778943089964E-16, 0.000000000000000000, 1.000000000000000000 ) ) ;
#3439 = CARTESIAN_POINT ( 'NONE',  ( 0.4974685680287860290, -5.439830508474580384, 7.000224381598740386 ) ) ;
#3440 = CARTESIAN_POINT ( 'NONE',  ( 1.250000000000000000, 6.144112549695430303, 5.100000000000000533 ) ) ;
#3441 = ADVANCED_FACE ( 'NONE', ( #17899, #5237, #6429 ), #4951, .T. ) ;
#3442 = CARTESIAN_POINT ( 'NONE',  ( 2.334748642087659753, -0.6593979156574648615, 4.403867486184822155 ) ) ;
#3443 = ADVANCED_FACE ( 'NONE', ( #791 ), #896, .F. ) ;
#3444 = CARTESIAN_POINT ( 'NONE',  ( -1.372722144827311475, -0.2742238837839081067, 2.407683403867349803 ) ) ;
#3445 = CARTESIAN_POINT ( 'NONE',  ( -1.008962495263940662, -4.614566048306495638, 7.154609617872592864 ) ) ;
#3446 = ORIENTED_EDGE ( 'NONE', *, *, #13244, .T. ) ;
#3447 = CARTESIAN_POINT ( 'NONE',  ( -2.075124426334559846, -2.918361879621429900, 5.810227140144559321 ) ) ;
#3448 = VECTOR ( 'NONE', #4761, 1000.000000000000000 ) ;
#3449 = LINE ( 'NONE', #6321, #17314 ) ;
#3450 = AXIS2_PLACEMENT_3D ( 'NONE', #1355, #7011, #12660 ) ;
#3451 = CARTESIAN_POINT ( 'NONE',  ( 1.800000000000000044, 12.00000000000000000, 7.649999999999999467 ) ) ;
#3452 = CARTESIAN_POINT ( 'NONE',  ( 2.013199450439951299, -3.873181699441240244, 5.102405038954985095 ) ) ;
#3453 = FACE_BOUND ( 'NONE', #18208, .T. ) ;
#3454 = CARTESIAN_POINT ( 'NONE',  ( 1.865240315818150973, -2.149848366107909303, 3.842223568244794496 ) ) ;
#3455 = ORIENTED_EDGE ( 'NONE', *, *, #5902, .F. ) ;
#3456 = LINE ( 'NONE', #10699, #7619 ) ;
#3457 = VECTOR ( 'NONE', #12795, 1000.000000000000000 ) ;
#3458 = VECTOR ( 'NONE', #14361, 1000.000000000000000 ) ;
#3459 = ADVANCED_FACE ( 'NONE', ( #10604 ), #7736, .F. ) ;
#3460 = DIRECTION ( 'NONE',  ( -1.000000000000000000, 0.000000000000000000, -2.220446049250309876E-16 ) ) ;
#3461 = CARTESIAN_POINT ( 'NONE',  ( -1.945845091386011250, -1.660794312053860633, 2.895339208235828909 ) ) ;
#3462 = EDGE_LOOP ( 'NONE', ( #13580, #13123, #13586, #6365 ) ) ;
#3463 = CARTESIAN_POINT ( 'NONE',  ( 1.800000000000000044, 0.5999999999999999778, 7.550000000000000711 ) ) ;
#3464 = LINE ( 'NONE', #14772, #11349 ) ;
#3465 = EDGE_CURVE ( 'NONE', #7904, #620, #3851, .T. ) ;
#3466 = FACE_OUTER_BOUND ( 'NONE', #9370, .T. ) ;
#3467 = CARTESIAN_POINT ( 'NONE',  ( -0.1565249325564300187, -5.153177966101689655, 7.048192310558509810 ) ) ;
#3468 = EDGE_LOOP ( 'NONE', ( #13484, #13630, #2931, #9071 ) ) ;
#3469 = EDGE_CURVE ( 'NONE', #15324, #12277, #5142, .T. ) ;
#3470 = VECTOR ( 'NONE', #9500, 1000.000000000000000 ) ;
#3471 = ORIENTED_EDGE ( 'NONE', *, *, #1518, .F. ) ;
#3472 = CARTESIAN_POINT ( 'NONE',  ( 1.899999999999999911, 7.299999999999999822, 1.600000000000000089 ) ) ;
#3473 = EDGE_CURVE ( 'NONE', #18021, #3042, #10793, .T. ) ;
#3474 = CYLINDRICAL_SURFACE ( 'NONE', #1686, 0.4000000000000000222 ) ;
#3475 = EDGE_CURVE ( 'NONE', #9567, #9752, #224, .T. ) ;
#3476 = EDGE_LOOP ( 'NONE', ( #3739, #10687, #14876, #9565 ) ) ;
#3477 = EDGE_CURVE ( 'NONE', #5262, #3744, #16257, .T. ) ;
#3478 = VECTOR ( 'NONE', #6449, 1000.000000000000000 ) ;
#3479 = CARTESIAN_POINT ( 'NONE',  ( 1.503451935564949826, -2.499172690432241772, 6.886949009567407742 ) ) ;
#3480 = SPHERICAL_SURFACE ( 'NONE', #14169, 1.016666666666670160 ) ;
#3481 = CARTESIAN_POINT ( 'NONE',  ( 1.094547058713730037, -2.844656138396588929, 7.117660114503893354 ) ) ;
#3482 = AXIS2_PLACEMENT_3D ( 'NONE', #8784, #4245, #5741 ) ;
#3483 = CARTESIAN_POINT ( 'NONE',  ( -0.1749999999999999889, 4.299999999999999822, 1.600000000000000089 ) ) ;
#3484 = CARTESIAN_POINT ( 'NONE',  ( 8.785293332290788772E-16, 10.80000000000000071, 7.599999999999999645 ) ) ;
#3485 = CARTESIAN_POINT ( 'NONE',  ( 1.044181395669780077, -3.547145663405210314, 2.590869634085890105 ) ) ;
#3486 = CARTESIAN_POINT ( 'NONE',  ( 1.149999999999999911, 6.472933199251450276, 6.846017351831609865 ) ) ;
#3487 = AXIS2_PLACEMENT_3D ( 'NONE', #17306, #477, #4904 ) ;
#3489 = ORIENTED_EDGE ( 'NONE', *, *, #7338, .T. ) ;
#3488 = CARTESIAN_POINT ( 'NONE',  ( 2.647661051184980519, -2.541908390648840665, 4.518328177639069132 ) ) ;
#3490 = DIRECTION ( 'NONE',  ( -3.315303352997239924E-31, 1.000000000000000000, -8.588360937600549480E-46 ) ) ;
#3491 = CARTESIAN_POINT ( 'NONE',  ( -2.328217775191430139, -0.5180084745762719711, 5.043379051721170292 ) ) ;
#3492 = CARTESIAN_POINT ( 'NONE',  ( -1.800000000000000044, 11.40000000000000036, 1.600000000000000089 ) ) ;
#3493 = VECTOR ( 'NONE', #13772, 1000.000000000000000 ) ;
#3494 = CARTESIAN_POINT ( 'NONE',  ( -1.417709711196470046, -2.006277760018209566, 2.821478011237799954 ) ) ;
#3495 = CARTESIAN_POINT ( 'NONE',  ( 2.345900685764729765, -0.3711864406779670222, 4.512231114381330066 ) ) ;
#3496 = AXIS2_PLACEMENT_3D ( 'NONE', #21, #11484, #1500 ) ;
#3497 = DIRECTION ( 'NONE',  ( 0.000000000000000000, -1.000000000000000000, 0.000000000000000000 ) ) ;
#3498 = CARTESIAN_POINT ( 'NONE',  ( -0.8570167067220350043, -5.582203389830509899, 2.508190348879359988 ) ) ;
#3499 = EDGE_LOOP ( 'NONE', ( #8353, #5809, #12333, #11809 ) ) ;
#3500 = EDGE_CURVE ( 'NONE', #15477, #5861, #13382, .T. ) ;
#3501 = CARTESIAN_POINT ( 'NONE',  ( -0.4000000000000000222, 2.399999999999999911, 6.100000000000000533 ) ) ;
#3502 = ORIENTED_EDGE ( 'NONE', *, *, #4388, .F. ) ;
#3503 = DIRECTION ( 'NONE',  ( -2.379049338482479710E-16, 0.000000000000000000, -1.000000000000000000 ) ) ;
#3504 = DIRECTION ( 'NONE',  ( 2.960594732333750117E-15, 2.960594732333750117E-15, -1.000000000000000000 ) ) ;
#3505 = AXIS2_PLACEMENT_3D ( 'NONE', #7084, #5688, #10122 ) ;
#3506 = VERTEX_POINT ( 'NONE', #2185 ) ;
#3507 = ORIENTED_EDGE ( 'NONE', *, *, #1665, .F. ) ;
#3508 = CARTESIAN_POINT ( 'NONE',  ( 2.211317922628870392, -2.472043525783979678, 3.894507149290419967 ) ) ;
#3509 = CARTESIAN_POINT ( 'NONE',  ( -2.116444151961480280, -5.546610169491529518, 3.670839500609359707 ) ) ;
#3510 = VECTOR ( 'NONE', #5815, 1000.000000000000000 ) ;
#3511 = EDGE_CURVE ( 'NONE', #17576, #6049, #12098, .T. ) ;
#3512 = CARTESIAN_POINT ( 'NONE',  ( -2.345213174852959881, -1.796683165423619943, 4.503223853122380049 ) ) ;
#3513 = CARTESIAN_POINT ( 'NONE',  ( -0.6864473529425049181, -4.591277760018209975, 6.951118770549909343 ) ) ;
#3514 = CARTESIAN_POINT ( 'NONE',  ( -2.045969882616350155, -1.796683165423619055, 4.529973290172065070 ) ) ;
#3515 = CARTESIAN_POINT ( 'NONE',  ( -2.500000000000000000, 4.700000000000000178, 1.600000000000000089 ) ) ;
#3516 = DIRECTION ( 'NONE',  ( -1.110223024625159992E-16, 0.000000000000000000, 1.000000000000000000 ) ) ;
#3517 = ORIENTED_EDGE ( 'NONE', *, *, #5755, .F. ) ;
#3518 = CARTESIAN_POINT ( 'NONE',  ( 1.558267747804329861, -0.7002976875533010181, 3.135138892994000059 ) ) ;
#3519 = EDGE_CURVE ( 'NONE', #435, #1178, #9301, .T. ) ;
#3520 = DIRECTION ( 'NONE',  ( -1.908195823574489776E-16, 1.000000000000000000, 6.938893903907229610E-17 ) ) ;
#3521 = CARTESIAN_POINT ( 'NONE',  ( -0.9485663501270049647, -3.054250732991179440, 6.853826262002260528 ) ) ;
#3522 = ORIENTED_EDGE ( 'NONE', *, *, #3477, .F. ) ;
#3523 = VECTOR ( 'NONE', #6288, 1000.000000000000000 ) ;
#3524 = ORIENTED_EDGE ( 'NONE', *, *, #13668, .T. ) ;
#3525 = DIRECTION ( 'NONE',  ( -1.000000000000000000, -4.014365738757630620E-15, -1.254489293361759815E-16 ) ) ;
#3526 = VERTEX_POINT ( 'NONE', #2279 ) ;
#3527 = PLANE ( 'NONE',  #3004 ) ;
#3528 = CARTESIAN_POINT ( 'NONE',  ( -0.7322514394120432923, -5.286652542372874741, 2.149183891723918993 ) ) ;
#3529 = CARTESIAN_POINT ( 'NONE',  ( -2.043308330018790198, -0.5002118644067800046, 5.867646457774669422 ) ) ;
#3530 = VERTEX_POINT ( 'NONE', #7933 ) ;
#3531 = DIRECTION ( 'NONE',  ( 1.000000000000000000, 0.000000000000000000, 0.000000000000000000 ) ) ;
#3532 = AXIS2_PLACEMENT_3D ( 'NONE', #16020, #6271, #10170 ) ;
#3533 = CARTESIAN_POINT ( 'NONE',  ( -0.2302241296435190154, -3.706322805063249959, 2.659926792304259990 ) ) ;
#3534 = CARTESIAN_POINT ( 'NONE',  ( 0.9664230948141925293, -0.01779661016949178609, 2.228384861502251457 ) ) ;
#3535 = ORIENTED_EDGE ( 'NONE', *, *, #7921, .T. ) ;
#3536 = CARTESIAN_POINT ( 'NONE',  ( 1.889104232906359870, -0.3444915254237289615, 3.296507079072520163 ) ) ;
#3537 = ORIENTED_EDGE ( 'NONE', *, *, #3623, .F. ) ;
#3538 = CARTESIAN_POINT ( 'NONE',  ( 2.560337424259670591, -0.06228813559322075172, 4.001768473655590519 ) ) ;
#3539 = VERTEX_POINT ( 'NONE', #9959 ) ;
#3540 = CARTESIAN_POINT ( 'NONE',  ( 1.899999999999999911, 0.5999999999999999778, 1.600000000000000089 ) ) ;
#3541 = LINE ( 'NONE', #14852, #6231 ) ;
#3542 = CIRCLE ( 'NONE', #10071, 0.6999999999999992895 ) ;
#3543 = CARTESIAN_POINT ( 'NONE',  ( -2.088297318559229954, -5.502118644067800268, 5.785136623276639689 ) ) ;
#3544 = CARTESIAN_POINT ( 'NONE',  ( 0.4500319419456214609, -4.474836318576761229, 7.315451193241913508 ) ) ;
#3545 = ORIENTED_EDGE ( 'NONE', *, *, #17166, .T. ) ;
#3546 = CARTESIAN_POINT ( 'NONE',  ( -1.209303714320900003, -4.865515740159329638, 2.662663894020049771 ) ) ;
#3547 = CARTESIAN_POINT ( 'NONE',  ( -0.5570002967655939274, -2.708767285026830063, 6.986590552960220357 ) ) ;
#3548 = CARTESIAN_POINT ( 'NONE',  ( 1.889999999999999902, 4.100000000000000533, 0.5999999999999999778 ) ) ;
#3549 = DIRECTION ( 'NONE',  ( 2.936127007273139866E-16, 0.000000000000000000, -1.000000000000000000 ) ) ;
#3550 = CARTESIAN_POINT ( 'NONE',  ( 2.021195349941390162, -3.780028546288090041, 4.339901124684640621 ) ) ;
#3551 = CARTESIAN_POINT ( 'NONE',  ( 0.1749999999999999889, 7.700000000000000178, 1.600000000000000089 ) ) ;
#3552 = CARTESIAN_POINT ( 'NONE',  ( 0.2335786437626899970, 6.450000000000000178, 1.958578643762689753 ) ) ;
#3553 = CARTESIAN_POINT ( 'NONE',  ( 1.992092870331701349, -2.196424942684489956, 4.203544726484164329 ) ) ;
#3554 = ORIENTED_EDGE ( 'NONE', *, *, #16644, .F. ) ;
#3555 = AXIS2_PLACEMENT_3D ( 'NONE', #14493, #13277, #1816 ) ;
#3556 = DIRECTION ( 'NONE',  ( 0.000000000000000000, -1.000000000000000000, 1.110223024625159992E-16 ) ) ;
#3557 = CARTESIAN_POINT ( 'NONE',  ( 0.5843165771433389555, -0.3612150962701970447, 2.403837883145309995 ) ) ;
#3558 = CARTESIAN_POINT ( 'NONE',  ( -2.212163452524020357, -2.895073591333140239, 6.166099093621881799 ) ) ;
#3559 = ORIENTED_EDGE ( 'NONE', *, *, #6783, .T. ) ;
#3560 = DIRECTION ( 'NONE',  ( -1.000000000000000000, 0.000000000000000000, 0.000000000000000000 ) ) ;
#3561 = CARTESIAN_POINT ( 'NONE',  ( -0.5902886515192680150, -1.447358841099289917, 6.978224088050050788 ) ) ;
#3562 = DIRECTION ( 'NONE',  ( -1.000000000000000000, 0.000000000000000000, 0.000000000000000000 ) ) ;
#3563 = CARTESIAN_POINT ( 'NONE',  ( -0.3743405594629430344, -5.157627118644070308, 7.023440622744399953 ) ) ;
#3564 = ORIENTED_EDGE ( 'NONE', *, *, #13003, .T. ) ;
#3565 = ORIENTED_EDGE ( 'NONE', *, *, #9873, .F. ) ;
#3566 = FACE_OUTER_BOUND ( 'NONE', #7105, .T. ) ;
#3567 = FACE_OUTER_BOUND ( 'NONE', #14925, .T. ) ;
#3568 = DIRECTION ( 'NONE',  ( 1.110223024625159992E-16, 4.440892098500630106E-16, -1.000000000000000000 ) ) ;
#3569 = ORIENTED_EDGE ( 'NONE', *, *, #16349, .T. ) ;
#3570 = CARTESIAN_POINT ( 'NONE',  ( -1.392553072310521278, -5.564406779661021041, 3.191531554476531252 ) ) ;
#3571 = CARTESIAN_POINT ( 'NONE',  ( -2.494165244384181079, -3.127956474216021299, 3.793218093085275910 ) ) ;
#3572 = CARTESIAN_POINT ( 'NONE',  ( 1.536215498768949361, -5.033893599512578199, 2.912754292501710918 ) ) ;
#3573 = CARTESIAN_POINT ( 'NONE',  ( 1.720450724489989813, -2.774791273531719060, 6.720683794561567836 ) ) ;
#3574 = EDGE_CURVE ( 'NONE', #7200, #15044, #10543, .T. ) ;
#3575 = DIRECTION ( 'NONE',  ( -2.960594732333750117E-16, -1.000000000000000000, 0.000000000000000000 ) ) ;
#3576 = PLANE ( 'NONE',  #1420 ) ;
#3577 = CARTESIAN_POINT ( 'NONE',  ( 1.552749016687789974, -4.036199717459258984, 6.468535037441730751 ) ) ;
#3578 = PRODUCT_DEFINITION ( 'UNKNOWN', '', #15377, #6775 ) ;
#3579 = EDGE_CURVE ( 'NONE', #2390, #13806, #8786, .T. ) ;
#3580 = CARTESIAN_POINT ( 'NONE',  ( -1.899999999999999911, 11.15000000000000036, 2.137972338849589826E-15 ) ) ;
#3581 = CARTESIAN_POINT ( 'NONE',  ( -0.1749999999999999889, 7.799999999999999822, 0.4000000000000000222 ) ) ;
#3583 = ORIENTED_EDGE ( 'NONE', *, *, #6705, .T. ) ;
#3582 = CARTESIAN_POINT ( 'NONE',  ( 2.282375681463800543, -2.425466949207401690, 3.345793611865401473 ) ) ;
#3584 = EDGE_CURVE ( 'NONE', #17897, #16690, #3933, .T. ) ;
#3585 = ADVANCED_FACE ( 'NONE', ( #1170 ), #6818, .F. ) ;
#3586 = DIRECTION ( 'NONE',  ( 1.110223024625159992E-16, 0.000000000000000000, -1.000000000000000000 ) ) ;
#3587 = CYLINDRICAL_SURFACE ( 'NONE', #2587, 0.4000000000000000222 ) ;
#3588 = CARTESIAN_POINT ( 'NONE',  ( -2.255259958075430227, -1.703530012270459970, 5.372717034856060003 ) ) ;
#3589 = CARTESIAN_POINT ( 'NONE',  ( -0.009452017499194409825, -5.299806473661739403, 2.336684903355700005 ) ) ;
#3590 = DIRECTION ( 'NONE',  ( -1.224646799147351975E-16, 1.000000000000000000, 6.123233995736750012E-17 ) ) ;
#3591 = CARTESIAN_POINT ( 'NONE',  ( -0.7983658734557950165, -5.466525423728810118, 6.913847129767330735 ) ) ;
#3592 = ORIENTED_EDGE ( 'NONE', *, *, #1546, .T. ) ;
#3593 = CARTESIAN_POINT ( 'NONE',  ( -0.9000000000000000222, 6.450000000000000178, 1.600000000000000089 ) ) ;
#3594 = ORIENTED_EDGE ( 'NONE', *, *, #17578, .T. ) ;
#3595 = CARTESIAN_POINT ( 'NONE',  ( 2.328217775191430139, -5.081991525423728895, 5.043379051721158746 ) ) ;
#3596 = LINE ( 'NONE', #13229, #15002 ) ;
#3597 = CARTESIAN_POINT ( 'NONE',  ( 0.1749999999999999889, 7.700000000000000178, 0.4000000000000000222 ) ) ;
#3598 = ORIENTED_EDGE ( 'NONE', *, *, #16143, .F. ) ;
#3599 = ORIENTED_EDGE ( 'NONE', *, *, #4595, .T. ) ;
#3600 = CARTESIAN_POINT ( 'NONE',  ( -1.669205944673819886, -3.147403886144329643, 6.359065158982450505 ) ) ;
#3601 = CARTESIAN_POINT ( 'NONE',  ( -1.899999999999999911, 4.700000000000000178, 1.600000000000000089 ) ) ;
#3602 = CARTESIAN_POINT ( 'NONE',  ( 2.224278379903029901, -5.390889830508481140, 5.468825643806100700 ) ) ;
#3603 = DIRECTION ( 'NONE',  ( -2.220446049250309876E-16, -1.000000000000000000, -1.479114197289400113E-30 ) ) ;
#3604 = EDGE_CURVE ( 'NONE', #13146, #389, #8393, .T. ) ;
#3605 = CARTESIAN_POINT ( 'NONE',  ( -1.586727176531439909, -1.982989471729919906, 2.961885344765640138 ) ) ;
#3606 = CARTESIAN_POINT ( 'NONE',  ( 0.6150581927482109412, -4.451548030288480895, 6.971662190339319665 ) ) ;
#3607 = VECTOR ( 'NONE', #15558, 1000.000000000000000 ) ;
#3608 = CARTESIAN_POINT ( 'NONE',  ( -1.966895454505930729, -1.703530012270459970, 5.288408118292069915 ) ) ;
#3609 = PLANE ( 'NONE',  #10566 ) ;
#3610 = VERTEX_POINT ( 'NONE', #188 ) ;
#3611 = CARTESIAN_POINT ( 'NONE',  ( 1.670747152266691016, -0.4963810343603142217, 3.047345280935851441 ) ) ;
#3612 = CARTESIAN_POINT ( 'NONE',  ( -0.5500000000000000444, 6.450000000000000178, 3.299999999999999822 ) ) ;
#3613 = CARTESIAN_POINT ( 'NONE',  ( 2.311987889326980294, -4.078935417675859654, 4.260161748947079552 ) ) ;
#3614 = ORIENTED_EDGE ( 'NONE', *, *, #11569, .T. ) ;
#3615 = ORIENTED_EDGE ( 'NONE', *, *, #12209, .T. ) ;
#3616 = DIRECTION ( 'NONE',  ( -1.899065700016719806E-16, -1.000000000000000000, 0.000000000000000000 ) ) ;
#3617 = ORIENTED_EDGE ( 'NONE', *, *, #16825, .T. ) ;
#3618 = DIRECTION ( 'NONE',  ( 1.110223024625159992E-16, 0.000000000000000000, -1.000000000000000000 ) ) ;
#3619 = CONTEXT_DEPENDENT_SHAPE_REPRESENTATION ( #8404, #4171 ) ;
#3620 = CARTESIAN_POINT ( 'NONE',  ( -3.188875856275119715E-15, -5.300000000000000711, 2.050000000000001155 ) ) ;
#3621 = PLANE ( 'NONE',  #11736 ) ;
#3622 = VERTEX_POINT ( 'NONE', #13053 ) ;
#3623 = EDGE_CURVE ( 'NONE', #10942, #15772, #15571, .T. ) ;
#3624 = LINE ( 'NONE', #8273, #7611 ) ;
#3625 = CARTESIAN_POINT ( 'NONE',  ( -1.423520578776781509, -3.543304787045241433, 3.220645071516951230 ) ) ;
#3626 = CARTESIAN_POINT ( 'NONE',  ( 1.800129581279440893, -0.03559322033898339871, 2.750028594811110061 ) ) ;
#3627 = ORIENTED_EDGE ( 'NONE', *, *, #1455, .T. ) ;
#3628 = CARTESIAN_POINT ( 'NONE',  ( 1.438959988998139914E-16, -0.2999999999999999889, 2.350000000000000089 ) ) ;
#3629 = CARTESIAN_POINT ( 'NONE',  ( 1.438959988998139914E-16, -2.775557561562889872E-16, 2.350000000000000089 ) ) ;
#3630 = ORIENTED_EDGE ( 'NONE', *, *, #11312, .T. ) ;
#3631 = CARTESIAN_POINT ( 'NONE',  ( -1.194742379459959869, -5.475423728813559876, 6.727584234649759409 ) ) ;
#3632 = CARTESIAN_POINT ( 'NONE',  ( 1.460675875430079484, -0.9155690868286360251, 6.545310725710027810 ) ) ;
#3633 = CARTESIAN_POINT ( 'NONE',  ( 1.811729841638690219, -5.341949152542369461, 3.197954009834290012 ) ) ;
#3634 = CARTESIAN_POINT ( 'NONE',  ( -2.408279507600840308, -4.800872354612795156, 5.815035204050404971 ) ) ;
#3635 = ORIENTED_EDGE ( 'NONE', *, *, #6228, .T. ) ;
#3636 = CARTESIAN_POINT ( 'NONE',  ( 2.241103642439659443E-15, 9.099999999999999645, 7.700000000000000178 ) ) ;
#3637 = CARTESIAN_POINT ( 'NONE',  ( -2.046174187462380445, -4.478677194936739880, 5.862719605944009871 ) ) ;
#3638 = ADVANCED_FACE ( 'NONE', ( #11393 ), #11656, .F. ) ;
#3639 = CARTESIAN_POINT ( 'NONE',  ( 1.750000000000000000, 0.5999999999999999778, 7.700000000000000178 ) ) ;
#3640 = CARTESIAN_POINT ( 'NONE',  ( -0.8014931112106958855, -4.315659176918716255, 6.590108630558016323 ) ) ;
#3641 = LINE ( 'NONE', #10493, #2306 ) ;
#3642 = CYLINDRICAL_SURFACE ( 'NONE', #2343, 0.6000000000000000888 ) ;
#3643 = CARTESIAN_POINT ( 'NONE',  ( 0.9588981328681075444, -1.986830348089900777, 2.884671871696430578 ) ) ;
#3644 = EDGE_LOOP ( 'NONE', ( #4944, #9300, #15904, #13361 ) ) ;
#3645 = DIRECTION ( 'NONE',  ( 0.000000000000000000, 0.000000000000000000, -1.000000000000000000 ) ) ;
#3646 = PLANE ( 'NONE',  #249 ) ;
#3647 =( REPRESENTATION_RELATIONSHIP ('NONE','NONE', #2757, #16473 ) REPRESENTATION_RELATIONSHIP_WITH_TRANSFORMATION ( #7702 )SHAPE_REPRESENTATION_RELATIONSHIP( ) );
#3648 = CARTESIAN_POINT ( 'NONE',  ( 1.652654650382400003, -0.7952867690272209522, 3.029252778805620050 ) ) ;
#3649 = CARTESIAN_POINT ( 'NONE',  ( 1.449852972479971358, -2.010118636378181112, 2.477154964647140911 ) ) ;
#3650 = ORIENTED_EDGE ( 'NONE', *, *, #12443, .F. ) ;
#3651 = CARTESIAN_POINT ( 'NONE',  ( 1.300000000000000044, -1.592040838891560081E-16, 7.599999999999999645 ) ) ;
#3652 = DIRECTION ( 'NONE',  ( 5.296209390990920866E-31, 1.000000000000000000, 8.548717289613711672E-15 ) ) ;
#3653 = DIRECTION ( 'NONE',  ( -4.177994306516039113E-17, 0.7310552682428709259, -0.6823182503600090376 ) ) ;
#3654 = CARTESIAN_POINT ( 'NONE',  ( -2.345900685764729765, -5.228813559322030180, 4.512231114381339836 ) ) ;
#3655 = ORIENTED_EDGE ( 'NONE', *, *, #14908, .F. ) ;
#3656 = ORIENTED_EDGE ( 'NONE', *, *, #5650, .F. ) ;
#3657 = LINE ( 'NONE', #5147, #4736 ) ;
#3658 = VECTOR ( 'NONE', #7986, 1000.000000000000000 ) ;
#3659 = DIRECTION ( 'NONE',  ( 3.700743415417190112E-16, 1.000000000000000000, -1.850371707708589879E-16 ) ) ;
#3660 = CARTESIAN_POINT ( 'NONE',  ( 2.500000000000000000, 7.299999999999999822, 1.600000000000000089 ) ) ;
#3661 = EDGE_LOOP ( 'NONE', ( #4569, #11417, #3419, #15550 ) ) ;
#3662 = CARTESIAN_POINT ( 'NONE',  ( -1.248294325655370018, -5.573305084745760141, 2.704938983774309857 ) ) ;
#3663 = ADVANCED_FACE ( 'NONE', ( #3059 ), #12964, .F. ) ;
#3664 = CARTESIAN_POINT ( 'NONE',  ( 0.1110902655589990351, -2.638902420161969520, 7.351560417169478612 ) ) ;
#3665 = CARTESIAN_POINT ( 'NONE',  ( -1.000000000000000000, -7.000000000000000000, 3.700000000000000178 ) ) ;
#3666 = CARTESIAN_POINT ( 'NONE',  ( 2.608006145151101407, -4.172088570829024512, 5.191342690854350295 ) ) ;
#3667 = LINE ( 'NONE', #2199, #11478 ) ;
#3668 = CARTESIAN_POINT ( 'NONE',  ( -2.500000000000000000, 2.000000000000000000, 2.755455298081550201E-16 ) ) ;
#3669 = CARTESIAN_POINT ( 'NONE',  ( 0.8429265834919229539, -3.523857375116919766, 2.502678798553439776 ) ) ;
#3670 = CARTESIAN_POINT ( 'NONE',  ( -3.061616997868380553E-17, 5.318248954186070243, 6.899999999999999467 ) ) ;
#3671 = LINE ( 'NONE', #8133, #12395 ) ;
#3673 = EDGE_LOOP ( 'NONE', ( #10875, #11329, #8025, #12193 ) ) ;
#3672 = CARTESIAN_POINT ( 'NONE',  ( 1.428323476796560465, -2.309025507765959606, 2.463260019887501429 ) ) ;
#3674 = AXIS2_PLACEMENT_3D ( 'NONE', #7767, #13412, #725 ) ;
#3675 = FACE_OUTER_BOUND ( 'NONE', #13560, .T. ) ;
#3676 = CARTESIAN_POINT ( 'NONE',  ( 1.248294325655350034, -0.3266949152542379942, 2.704938983774300088 ) ) ;
#3677 = CARTESIAN_POINT ( 'NONE',  ( 0.06276132972186961034, -1.377493976234430040, 7.052616990284530374 ) ) ;
#3678 = CARTESIAN_POINT ( 'NONE',  ( -0.9150601050661559821, -0.4690677966101700069, 6.868218666554230190 ) ) ;
#3679 = CARTESIAN_POINT ( 'NONE',  ( -0.9000000000000000222, -9.500000000000000000, 8.099999999999999645 ) ) ;
#3680 = ORIENTED_EDGE ( 'NONE', *, *, #8960, .T. ) ;
#3681 = CARTESIAN_POINT ( 'NONE',  ( -1.399999999999999911, 5.799999999999999822, 7.700000000000000178 ) ) ;
#3682 = ORIENTED_EDGE ( 'NONE', *, *, #12918, .F. ) ;
#3683 = CARTESIAN_POINT ( 'NONE',  ( 2.143090896833109493, -5.095338983050849535, 5.672454929438340621 ) ) ;
#3684 = LINE ( 'NONE', #1852, #1405 ) ;
#3685 = CARTESIAN_POINT ( 'NONE',  ( -1.399999999999999911, -9.500000000000000000, 3.299999999999999822 ) ) ;
#3686 = EDGE_CURVE ( 'NONE', #4246, #3854, #1764, .T. ) ;
#3687 = ORIENTED_EDGE ( 'NONE', *, *, #4124, .T. ) ;
#3688 = EDGE_CURVE ( 'NONE', #14447, #2805, #8881, .T. ) ;
#3689 = CARTESIAN_POINT ( 'NONE',  ( 1.444955263746720009, -2.332313796054249710, 2.842353646881480511 ) ) ;
#3690 = CARTESIAN_POINT ( 'NONE',  ( 2.220446049250309876E-16, 2.399999999999999911, 6.100000000000000533 ) ) ;
#3691 = CARTESIAN_POINT ( 'NONE',  ( 0.5500000000000000444, 3.050000000000000266, 3.299999999999999822 ) ) ;
#3692 = CARTESIAN_POINT ( 'NONE',  ( 1.526791597786429922, -2.774791273531720392, 6.490992212270249695 ) ) ;
#3693 = AXIS2_PLACEMENT_3D ( 'NONE', #10327, #1898, #17705 ) ;
#3694 = CARTESIAN_POINT ( 'NONE',  ( -1.889999999999999902, 7.900000000000000355, 3.000000000000000000 ) ) ;
#3695 = CARTESIAN_POINT ( 'NONE',  ( -0.1781895581254780980, -2.146007489747939090, 2.654724878163539969 ) ) ;
#3696 = LINE ( 'NONE', #10745, #7910 ) ;
#3697 = CARTESIAN_POINT ( 'NONE',  ( 2.500000000000000000, 9.199999999999999289, 1.600000000000000089 ) ) ;
#3698 = EDGE_LOOP ( 'NONE', ( #16861, #3569, #17508, #9473 ) ) ;
#3699 = VECTOR ( 'NONE', #6516, 1000.000000000000000 ) ;
#3700 = CARTESIAN_POINT ( 'NONE',  ( -1.550000000000000044, -5.599999999999999645, 6.100000000000000533 ) ) ;
#3701 = CARTESIAN_POINT ( 'NONE',  ( -1.914021115237000137, -4.754295778036220277, 6.069404563272239983 ) ) ;
#3702 = ORIENTED_EDGE ( 'NONE', *, *, #9850, .F. ) ;
#3703 = ORIENTED_EDGE ( 'NONE', *, *, #90, .T. ) ;
#3704 = ADVANCED_FACE ( 'NONE', ( #15930 ), #3239, .F. ) ;
#3705 = ORIENTED_EDGE ( 'NONE', *, *, #6178, .T. ) ;
#3706 = DIRECTION ( 'NONE',  ( 1.059690869644410208E-14, 1.000000000000000000, -1.027162637006522002E-32 ) ) ;
#3707 = ADVANCED_FACE ( 'NONE', ( #2215 ), #15600, .T. ) ;
#3708 = CARTESIAN_POINT ( 'NONE',  ( -0.08231150243516484333, -5.298516949152545230, 2.050000000000001155 ) ) ;
#3709 = DIRECTION ( 'NONE',  ( 1.000000000000000000, 0.000000000000000000, 0.000000000000000000 ) ) ;
#3710 = EDGE_LOOP ( 'NONE', ( #8903, #4722, #13648, #13411 ) ) ;
#3711 = AXIS2_PLACEMENT_3D ( 'NONE', #17892, #6615, #5042 ) ;
#3712 = CARTESIAN_POINT ( 'NONE',  ( 0.03714311608463249925, -1.078587104846649991, 7.053160869216429596 ) ) ;
#3713 = DIRECTION ( 'NONE',  ( 0.000000000000000000, -1.000000000000000000, 0.000000000000000000 ) ) ;
#3714 = CARTESIAN_POINT ( 'NONE',  ( -2.199335452462570117, -1.866548030288480042, 3.862342996790939953 ) ) ;
#3715 = CARTESIAN_POINT ( 'NONE',  ( -2.416676968769249090, -0.2046610169491529518, 5.796598111919839980 ) ) ;
#3716 = VERTEX_POINT ( 'NONE', #16024 ) ;
#3717 = ORIENTED_EDGE ( 'NONE', *, *, #2565, .T. ) ;
#3718 = CARTESIAN_POINT ( 'NONE',  ( 1.747582379783020778, -0.1156779661016950206, 6.697200745122486865 ) ) ;
#3719 = ORIENTED_EDGE ( 'NONE', *, *, #8897, .T. ) ;
#3720 = CARTESIAN_POINT ( 'NONE',  ( 1.661700935665417544, -5.037501140877957084, 3.038299064334577082 ) ) ;
#3721 = FACE_OUTER_BOUND ( 'NONE', #5602, .T. ) ;
#3722 = EDGE_CURVE ( 'NONE', #1331, #5830, #7677, .T. ) ;
#3723 = AXIS2_PLACEMENT_3D ( 'NONE', #3548, #9195, #5130 ) ;
#3724 = CARTESIAN_POINT ( 'NONE',  ( 0.4735094604799088280, -1.032010528270080219, 7.005327412390689901 ) ) ;
#3725 = CARTESIAN_POINT ( 'NONE',  ( -0.3743405594629430344, -5.457627118644070130, 7.023440622744399953 ) ) ;
#3726 = CARTESIAN_POINT ( 'NONE',  ( 2.006003143956041068, -0.8689925102520592581, 6.437545705712618194 ) ) ;
#3727 = VERTEX_POINT ( 'NONE', #10643 ) ;
#3728 = DIRECTION ( 'NONE',  ( 1.000000000000000000, 0.000000000000000000, 0.000000000000000000 ) ) ;
#3729 = CARTESIAN_POINT ( 'NONE',  ( -2.231116159141639965, -4.688271789531330391, 3.951089877392499616 ) ) ;
#3730 = CARTESIAN_POINT ( 'NONE',  ( 1.579331079541870686, -4.358394877135324030, 6.832797935622368257 ) ) ;
#3731 = CARTESIAN_POINT ( 'NONE',  ( 1.000000000000000000, -5.000000000000000000, 3.299999999999999822 ) ) ;
#3732 = DIRECTION ( 'NONE',  ( 1.000000000000000000, 0.000000000000000000, 0.000000000000000000 ) ) ;
#3733 = VECTOR ( 'NONE', #5842, 1000.000000000000000 ) ;
#3734 = CARTESIAN_POINT ( 'NONE',  ( 1.903446074666960364, -3.919758276017824006, 5.469282057156545029 ) ) ;
#3735 = CARTESIAN_POINT ( 'NONE',  ( -0.5500000000000000444, 6.450000000000000178, 3.200000000000000178 ) ) ;
#3736 = PLANE ( 'NONE',  #4405 ) ;
#3737 = AXIS2_PLACEMENT_3D ( 'NONE', #16748, #1293, #4157 ) ;
#3738 = CARTESIAN_POINT ( 'NONE',  ( -2.018065005288401270, -1.427911429170979352, 5.077247235985114848 ) ) ;
#3739 = ORIENTED_EDGE ( 'NONE', *, *, #14920, .T. ) ;
#3740 = DIRECTION ( 'NONE',  ( -1.048990684667790150E-15, 1.966625170870250139E-17, -1.000000000000000000 ) ) ;
#3741 = DIRECTION ( 'NONE',  ( 1.000000000000000000, 0.000000000000000000, 0.000000000000000000 ) ) ;
#3742 = PLANE ( 'NONE',  #14732 ) ;
#3743 = CARTESIAN_POINT ( 'NONE',  ( -2.594645788401189090, -2.988226744486289999, 5.257608218854294968 ) ) ;
#3744 = VERTEX_POINT ( 'NONE', #14531 ) ;
#3745 = LINE ( 'NONE', #3463, #6436 ) ;
#3746 = AXIS2_PLACEMENT_3D ( 'NONE', #9139, #15098, #10725 ) ;
#3747 = VECTOR ( 'NONE', #17361, 1000.000000000000000 ) ;
#3748 = CARTESIAN_POINT ( 'NONE',  ( 1.850000000000000089, -5.599999999999999645, 2.799999999999999822 ) ) ;
#3749 = CARTESIAN_POINT ( 'NONE',  ( 1.289141334274990447, -5.117584745762705722, 6.297747079672416426 ) ) ;
#3750 = ORIENTED_EDGE ( 'NONE', *, *, #7232, .T. ) ;
#3751 = EDGE_CURVE ( 'NONE', #11239, #7262, #18207, .T. ) ;
#3752 = ORIENTED_EDGE ( 'NONE', *, *, #10639, .F. ) ;
#3753 = PLANE ( 'NONE',  #18038 ) ;
#3754 = CARTESIAN_POINT ( 'NONE',  ( -1.652654650382402668, -4.804713230972782689, 3.029252778805632484 ) ) ;
#3755 = CARTESIAN_POINT ( 'NONE',  ( -1.000000000000000000, -5.500000000000000000, 6.100000000000000533 ) ) ;
#3756 = ORIENTED_EDGE ( 'NONE', *, *, #8364, .T. ) ;
#3757 = CIRCLE ( 'NONE', #501, 0.2500000000000002220 ) ;
#3758 = CARTESIAN_POINT ( 'NONE',  ( 1.943632316591230147, -5.346398305084740343, 3.373048379518159834 ) ) ;
#3759 = CARTESIAN_POINT ( 'NONE',  ( 2.639965200365849363, -3.849893411152959910, 4.971472712918224346 ) ) ;
#3760 = LINE ( 'NONE', #9423, #13888 ) ;
#3761 = CARTESIAN_POINT ( 'NONE',  ( -2.435897774776361491, -3.240557039297494057, 5.753335522918235689 ) ) ;
#3762 = LINE ( 'NONE', #3387, #8235 ) ;
#3763 = CARTESIAN_POINT ( 'NONE',  ( 0.1749999999999999889, 4.299999999999999822, 0.5999999999999999778 ) ) ;
#3764 = AXIS2_PLACEMENT_3D ( 'NONE', #16684, #6873, #14935 ) ;
#3765 = CARTESIAN_POINT ( 'NONE',  ( 0.4201920264139500372, -3.477280798540340001, 2.384360920086630031 ) ) ;
#3766 = AXIS2_PLACEMENT_3D ( 'NONE', #3901, #15214, #18048 ) ;
#3767 = VECTOR ( 'NONE', #14107, 1000.000000000000000 ) ;
#3768 = DIRECTION ( 'NONE',  ( 1.000000000000000000, 0.000000000000000000, -2.220446049250309876E-16 ) ) ;
#3769 = CARTESIAN_POINT ( 'NONE',  ( -1.300000000000000044, 1.592040838891560081E-16, 7.700000000000000178 ) ) ;
#3771 = ORIENTED_EDGE ( 'NONE', *, *, #34, .F. ) ;
#3770 = CARTESIAN_POINT ( 'NONE',  ( 2.653064503426820764, -2.565196678937129438, 4.766048721853534786 ) ) ;
#3772 = VECTOR ( 'NONE', #3741, 1000.000000000000000 ) ;
#3773 = DIRECTION ( 'NONE',  ( 2.220446049250309876E-16, 1.000000000000000000, 0.000000000000000000 ) ) ;
#3774 = VECTOR ( 'NONE', #4566, 1000.000000000000000 ) ;
#3775 = CARTESIAN_POINT ( 'NONE',  ( 1.889104232906359870, -0.3444915254237289615, 3.296507079072520163 ) ) ;
#3776 = CARTESIAN_POINT ( 'NONE',  ( -0.3752419433106839453, -1.424070552810999812, 7.023346545710370314 ) ) ;
#3777 = LINE ( 'NONE', #9609, #11025 ) ;
#3778 = ADVANCED_BREP_SHAPE_REPRESENTATION ( '', ( #1903, #17681 ), #4992 ) ;
#3779 = CARTESIAN_POINT ( 'NONE',  ( 1.850000000000000089, -5.599999999999999645, 6.899999999999999467 ) ) ;
#3780 = CARTESIAN_POINT ( 'NONE',  ( -0.5889081234606770021, -5.462076271186440124, 6.978529000034869867 ) ) ;
#3781 = ORIENTED_EDGE ( 'NONE', *, *, #9002, .F. ) ;
#3782 = VERTEX_POINT ( 'NONE', #14808 ) ;
#3783 = CYLINDRICAL_SURFACE ( 'NONE', #6371, 0.2000000000000000389 ) ;
#3784 = DIRECTION ( 'NONE',  ( -1.850371707708589879E-16, -1.000000000000000000, 0.000000000000000000 ) ) ;
#3786 = VECTOR ( 'NONE', #15237, 1000.000000000000000 ) ;
#3785 = AXIS2_PLACEMENT_3D ( 'NONE', #11468, #8774, #7482 ) ;
#3787 = VERTEX_POINT ( 'NONE', #4706 ) ;
#3788 = CARTESIAN_POINT ( 'NONE',  ( -2.295719155670160383, -3.287133615874060055, 5.218091927917240191 ) ) ;
#3789 = VECTOR ( 'NONE', #15857, 1000.000000000000000 ) ;
#3790 = CARTESIAN_POINT ( 'NONE',  ( 1.800000000000000044, 7.799999999999999822, 1.600000000000000089 ) ) ;
#3791 = CARTESIAN_POINT ( 'NONE',  ( 1.300961508564179914, -5.422033898305079092, 6.661123742937279602 ) ) ;
#3792 = CARTESIAN_POINT ( 'NONE',  ( -1.800000000000000044, 11.29999999999999893, 7.649999999999999467 ) ) ;
#3793 = FACE_OUTER_BOUND ( 'NONE', #16966, .T. ) ;
#3794 = CARTESIAN_POINT ( 'NONE',  ( -1.417709711196470046, -2.006277760018209566, 2.821478011237799954 ) ) ;
#3795 = VECTOR ( 'NONE', #2109, 1000.000000000000000 ) ;
#3796 = DIRECTION ( 'NONE',  ( 0.000000000000000000, -1.000000000000000000, 0.000000000000000000 ) ) ;
#3797 = VECTOR ( 'NONE', #17158, 1000.000000000000000 ) ;
#3798 = CARTESIAN_POINT ( 'NONE',  ( 1.985741519624368845, -2.495331814072259569, 4.178720363079467148 ) ) ;
#3799 = AXIS2_PLACEMENT_3D ( 'NONE', #8834, #4912, #2054 ) ;
#3800 = CARTESIAN_POINT ( 'NONE',  ( -0.4974685680287780354, -0.4601694915254240237, 7.000224381598740386 ) ) ;
#3801 = CARTESIAN_POINT ( 'NONE',  ( 1.300000000000000044, -1.592040838891560081E-16, 7.700000000000000178 ) ) ;
#3802 = ADVANCED_FACE ( 'NONE', ( #2118 ), #6193, .T. ) ;
#3803 = CARTESIAN_POINT ( 'NONE',  ( -1.449568901432419343, -0.2625000000000002331, 3.250431098567584165 ) ) ;
#3804 = ORIENTED_EDGE ( 'NONE', *, *, #17656, .T. ) ;
#3805 = AXIS2_PLACEMENT_3D ( 'NONE', #4192, #1151, #8458 ) ;
#3806 = DIRECTION ( 'NONE',  ( 0.000000000000000000, -0.2588190451025180749, 0.9659258262890690894 ) ) ;
#3807 = CARTESIAN_POINT ( 'NONE',  ( -0.5500000000000000444, 2.050000000000000266, 3.600000000000000089 ) ) ;
#3808 = ORIENTED_EDGE ( 'NONE', *, *, #16592, .F. ) ;
#3809 = VERTEX_POINT ( 'NONE', #16194 ) ;
#3810 = PRODUCT_DEFINITION_CONTEXT ( 'detailed design', #7117, 'design' ) ;
#3811 = ORIENTED_EDGE ( 'NONE', *, *, #1114, .F. ) ;
#3812 = LINE ( 'NONE', #6385, #11862 ) ;
#3813 = VECTOR ( 'NONE', #7499, 1000.000000000000000 ) ;
#3814 = CARTESIAN_POINT ( 'NONE',  ( -2.116444151961480280, -5.246610169491529696, 3.670839500609359707 ) ) ;
#3815 = CARTESIAN_POINT ( 'NONE',  ( -1.399999999999999911, 0.5999999999999999778, 3.299999999999999822 ) ) ;
#3816 = EDGE_LOOP ( 'NONE', ( #12509, #16636, #15774, #6623 ) ) ;
#3817 = CARTESIAN_POINT ( 'NONE',  ( -2.426866425021068974, -4.711560077819614278, 3.626019996130659617 ) ) ;
#3818 =( GEOMETRIC_REPRESENTATION_CONTEXT ( 3 ) GLOBAL_UNCERTAINTY_ASSIGNED_CONTEXT ( ( #9551 ) ) GLOBAL_UNIT_ASSIGNED_CONTEXT ( ( #1746, #270, #12852 ) ) REPRESENTATION_CONTEXT ( 'NONE', 'WORKASPACE' ) );
#3819 = ADVANCED_FACE ( 'NONE', ( #10733 ), #11849, .F. ) ;
#3820 = DIRECTION ( 'NONE',  ( 1.000000000000000000, 0.000000000000000000, 0.000000000000000000 ) ) ;
#3821 = CARTESIAN_POINT ( 'NONE',  ( -1.953802435660519921, -4.987178660919110662, 4.069478085301024173 ) ) ;
#3822 = ADVANCED_FACE ( 'NONE', ( #12029 ), #4791, .F. ) ;
#3823 = CARTESIAN_POINT ( 'NONE',  ( 2.203023580853990193, -0.05783898305084790581, 3.872235369154280349 ) ) ;
#3824 = VERTEX_POINT ( 'NONE', #3399 ) ;
#3825 = CARTESIAN_POINT ( 'NONE',  ( 2.340070819011249803, -0.3800847457627120063, 4.950151441910540129 ) ) ;
#3826 = EDGE_CURVE ( 'NONE', #11926, #3897, #3596, .T. ) ;
#3827 = AXIS2_PLACEMENT_3D ( 'NONE', #16541, #120, #16877 ) ;
#3828 = EDGE_CURVE ( 'NONE', #13806, #10942, #13414, .T. ) ;
#3829 = ORIENTED_EDGE ( 'NONE', *, *, #8105, .T. ) ;
#3830 = VERTEX_POINT ( 'NONE', #13143 ) ;
#3831 = DIRECTION ( 'NONE',  ( 0.000000000000000000, -1.000000000000000000, 0.000000000000000000 ) ) ;
#3832 = CARTESIAN_POINT ( 'NONE',  ( -0.6150581927481592048, -1.148451969711520082, 6.971662190339330323 ) ) ;
#3833 = CARTESIAN_POINT ( 'NONE',  ( 0.2812789908084389889, -5.444279661016950378, 7.036533610117280624 ) ) ;
#3834 = CARTESIAN_POINT ( 'NONE',  ( -1.947945325730720434, -1.288181699441250050, 6.502393603230366637 ) ) ;
#3835 = ORIENTED_EDGE ( 'NONE', *, *, #528, .F. ) ;
#3836 = LINE ( 'NONE', #10876, #18177 ) ;
#3837 = AXIS2_PLACEMENT_3D ( 'NONE', #17277, #10257, #4787 ) ;
#3838 = CARTESIAN_POINT ( 'NONE',  ( -1.303621121494419999, -4.362235753495300905, 6.659417683669699883 ) ) ;
#3839 = ADVANCED_FACE ( 'NONE', ( #12130 ), #827, .T. ) ;
#3840 = CARTESIAN_POINT ( 'NONE',  ( -1.875000000000000000, 0.7500000000000000000, 8.300000000000000711 ) ) ;
#3841 = CARTESIAN_POINT ( 'NONE',  ( 2.050563521385710075, -1.004881363621820567, 4.800454404529174823 ) ) ;
#3843 = EDGE_CURVE ( 'NONE', #12574, #14329, #6363, .T. ) ;
#3842 = DIRECTION ( 'NONE',  ( -0.000000000000000000, 1.000000000000000000, 0.000000000000000000 ) ) ;
#3844 = ORIENTED_EDGE ( 'NONE', *, *, #17696, .T. ) ;
#3845 = DIRECTION ( 'NONE',  ( 1.000000000000000000, 0.000000000000000000, 0.000000000000000000 ) ) ;
#3846 = DIRECTION ( 'NONE',  ( -2.478176394252584099E-15, 1.000000000000000000, 0.000000000000000000 ) ) ;
#3847 = CARTESIAN_POINT ( 'NONE',  ( 1.392553072310509510, -0.3355932203389832558, 3.191531554476519261 ) ) ;
#3848 = CARTESIAN_POINT ( 'NONE',  ( 3.179896940101190659E-17, 3.786446520921940007, 7.919316580472860245 ) ) ;
#3849 = CARTESIAN_POINT ( 'NONE',  ( 2.652303127816839190, -2.266289807549351387, 4.791661394135748431 ) ) ;
#3850 = AXIS2_PLACEMENT_3D ( 'NONE', #3303, #15902, #265 ) ;
#3851 = LINE ( 'NONE', #7828, #4055 ) ;
#3852 = CYLINDRICAL_SURFACE ( 'NONE', #595, 0.3499999999999999778 ) ;
#3853 = CARTESIAN_POINT ( 'NONE',  ( 1.695509042132770761, -5.346398305084745672, 3.542446458728613301 ) ) ;
#3854 = VERTEX_POINT ( 'NONE', #16379 ) ;
#3855 = CARTESIAN_POINT ( 'NONE',  ( 1.850000000000000089, -5.599999999999999645, 6.899999999999999467 ) ) ;
#3856 = CARTESIAN_POINT ( 'NONE',  ( 2.332582362116870200, -5.368644067796609853, 4.387643303570810005 ) ) ;
#3857 = DIRECTION ( 'NONE',  ( 1.000000000000000000, 0.000000000000000000, 0.000000000000000000 ) ) ;
#3858 = ORIENTED_EDGE ( 'NONE', *, *, #17628, .F. ) ;
#3859 = CARTESIAN_POINT ( 'NONE',  ( -1.194742379459959869, -5.475423728813559876, 6.727584234649759409 ) ) ;
#3860 = CARTESIAN_POINT ( 'NONE',  ( -2.626509418457480649, -4.571830348089889640, 5.080213055741825023 ) ) ;
#3861 = DIRECTION ( 'NONE',  ( -1.054711873393900133E-14, -1.000000000000000000, 0.000000000000000000 ) ) ;
#3862 = CARTESIAN_POINT ( 'NONE',  ( 1.899999999999999911, 11.40000000000000036, 0.5999999999999999778 ) ) ;
#3863 = VECTOR ( 'NONE', #6539, 1000.000000000000000 ) ;
#3864 = CARTESIAN_POINT ( 'NONE',  ( -2.053221424930790295, -4.734848366107910600, 3.549770689668290125 ) ) ;
#3866 = EDGE_CURVE ( 'NONE', #1371, #14390, #3684, .T. ) ;
#3865 = DIRECTION ( 'NONE',  ( 0.000000000000000000, -1.000000000000000000, 0.000000000000000000 ) ) ;
#3867 = LINE ( 'NONE', #3581, #4101 ) ;
#3869 = ORIENTED_EDGE ( 'NONE', *, *, #18169, .F. ) ;
#3868 = CARTESIAN_POINT ( 'NONE',  ( 2.619177996481910853, -2.518620102360551893, 4.272191262657148769 ) ) ;
#3870 = DIRECTION ( 'NONE',  ( 0.000000000000000000, 1.000000000000000000, 1.665334536937730077E-15 ) ) ;
#3871 = CARTESIAN_POINT ( 'NONE',  ( 1.978267656359410154, -0.4023305084745769644, 5.974740860598790171 ) ) ;
#3872 = CARTESIAN_POINT ( 'NONE',  ( 0.4985810152601650724, -1.330917399657850053, 7.000035360316460675 ) ) ;
#3873 = LINE ( 'NONE', #10727, #13380 ) ;
#3874 = FACE_OUTER_BOUND ( 'NONE', #13904, .T. ) ;
#3875 = CARTESIAN_POINT ( 'NONE',  ( 1.932035991685901122, -5.038983050847454237, 2.884370051397200818 ) ) ;
#3876 = ORIENTED_EDGE ( 'NONE', *, *, #12580, .F. ) ;
#3877 = PRODUCT_DEFINITION_SHAPE ( 'NONE', 'NONE',  #18292 ) ;
#3878 = ORIENTED_EDGE ( 'NONE', *, *, #13264, .T. ) ;
#3879 = CARTESIAN_POINT ( 'NONE',  ( 4.225031457058369810E-16, 2.299999999999999822, 7.599999999999999645 ) ) ;
#3880 = AXIS2_PLACEMENT_3D ( 'NONE', #4906, #17861, #13537 ) ;
#3881 = DIRECTION ( 'NONE',  ( -1.000000000000000000, 0.000000000000000000, 0.000000000000000000 ) ) ;
#3882 = VERTEX_POINT ( 'NONE', #7496 ) ;
#3883 = CARTESIAN_POINT ( 'NONE',  ( 2.262450597846779932, -4.195376859117310175, 5.348122657979680561 ) ) ;
#3884 = DIRECTION ( 'NONE',  ( 1.000000000000000000, 0.000000000000000000, -4.265713465516738421E-15 ) ) ;
#3885 = CARTESIAN_POINT ( 'NONE',  ( -2.270487904532170198, -5.537711864406779760, 4.080813552109679776 ) ) ;
#3886 = FACE_OUTER_BOUND ( 'NONE', #11950, .T. ) ;
#3887 = DIRECTION ( 'NONE',  ( -2.993800930630270167E-16, -6.049014748177290126E-16, 1.000000000000000000 ) ) ;
#3888 = CARTESIAN_POINT ( 'NONE',  ( -2.062913653388399826, -3.217268751009200400, 5.832754583370829415 ) ) ;
#3889 = CARTESIAN_POINT ( 'NONE',  ( 0.9000000000000000222, -10.00000000000000000, 6.100000000000000533 ) ) ;
#3890 = CARTESIAN_POINT ( 'NONE',  ( -0.6965028529798926726, -1.470647129387581575, 6.631265289497783044 ) ) ;
#3891 = LINE ( 'NONE', #6767, #12961 ) ;
#3892 = DIRECTION ( 'NONE',  ( -1.000000000000000000, 1.776356839399099990E-14, 0.000000000000000000 ) ) ;
#3893 = ORIENTED_EDGE ( 'NONE', *, *, #11288, .F. ) ;
#3894 = LINE ( 'NONE', #17669, #15803 ) ;
#3895 =( NAMED_UNIT ( * ) SI_UNIT ( $, .STERADIAN. ) SOLID_ANGLE_UNIT ( ) );
#3896 = VERTEX_POINT ( 'NONE', #3324 ) ;
#3897 = VERTEX_POINT ( 'NONE', #456 ) ;
#3898 = ORIENTED_EDGE ( 'NONE', *, *, #6448, .F. ) ;
#3899 = LINE ( 'NONE', #15302, #15653 ) ;
#3900 = CARTESIAN_POINT ( 'NONE',  ( -1.248294325655370018, -5.273305084745760318, 2.704938983774309857 ) ) ;
#3901 = CARTESIAN_POINT ( 'NONE',  ( 1.889999999999999902, 4.100000000000000533, 0.5999999999999999778 ) ) ;
#3902 = DIRECTION ( 'NONE',  ( 0.000000000000000000, 0.000000000000000000, -1.000000000000000000 ) ) ;
#3903 = CARTESIAN_POINT ( 'NONE',  ( 1.282210379528780031, -0.9388573751169240200, 6.673494927815259992 ) ) ;
#3904 = CARTESIAN_POINT ( 'NONE',  ( -1.850000000000000089, -5.599999999999999645, 2.299999999999999822 ) ) ;
#3905 = CARTESIAN_POINT ( 'NONE',  ( -1.981271652668300298, -1.633665147405599871, 5.970160748022450115 ) ) ;
#3906 = CARTESIAN_POINT ( 'NONE',  ( 1.194742379459969861, -0.1245762711864410038, 6.727584234649759409 ) ) ;
#3907 = ORIENTED_EDGE ( 'NONE', *, *, #1258, .F. ) ;
#3908 = CARTESIAN_POINT ( 'NONE',  ( 0.1565249325564390115, -0.4468220338983060480, 7.048192310558509810 ) ) ;
#3909 = ORIENTED_EDGE ( 'NONE', *, *, #1782, .T. ) ;
#3910 = CARTESIAN_POINT ( 'NONE',  ( 1.057242234132090175, -0.02224576271186469792, 2.597442975781520058 ) ) ;
#3911 = EDGE_LOOP ( 'NONE', ( #6196, #3598, #13942, #13403 ) ) ;
#3912 = CARTESIAN_POINT ( 'NONE',  ( -1.599999999999869971, 12.00000000000000000, 1.600000000000000089 ) ) ;
#3913 = CARTESIAN_POINT ( 'NONE',  ( 0.7435598031058588964, -2.569037555297099651, 6.932904947974519949 ) ) ;
#3914 = CARTESIAN_POINT ( 'NONE',  ( -1.194742379459959869, -5.475423728813559876, 6.727584234649759409 ) ) ;
#3915 = EDGE_CURVE ( 'NONE', #7890, #1801, #13319, .T. ) ;
#3916 = CARTESIAN_POINT ( 'NONE',  ( -2.642463257358080853, -1.451199717459271454, 4.945970783863430142 ) ) ;
#3917 = VERTEX_POINT ( 'NONE', #11756 ) ;
#3918 = CARTESIAN_POINT ( 'NONE',  ( -0.4649462444738060030, -5.251463457376920552, 2.383584851084299849 ) ) ;
#3919 = AXIS2_PLACEMENT_3D ( 'NONE', #2465, #6713, #13749 ) ;
#3920 = EDGE_CURVE ( 'NONE', #3809, #14294, #17386, .T. ) ;
#3921 = CARTESIAN_POINT ( 'NONE',  ( 2.308170020371300257, -3.873181699441239800, 5.159452766389609479 ) ) ;
#3922 = ADVANCED_FACE ( 'NONE', ( #9332 ), #12489, .F. ) ;
#3923 = CARTESIAN_POINT ( 'NONE',  ( -1.882879255550339082, -5.103620102360555855, 2.835213315261639000 ) ) ;
#3924 = FACE_OUTER_BOUND ( 'NONE', #11029, .T. ) ;
#3925 = PLANE ( 'NONE',  #2547 ) ;
#3926 = CARTESIAN_POINT ( 'NONE',  ( -1.899999999999999911, 3.500000000000000000, 0.6099999999999999867 ) ) ;
#3927 = CARTESIAN_POINT ( 'NONE',  ( -2.050994839075679366, -4.618406924666464519, 4.608774933727191048 ) ) ;
#3928 = LINE ( 'NONE', #6896, #14418 ) ;
#3929 = ORIENTED_EDGE ( 'NONE', *, *, #9982, .T. ) ;
#3930 = CARTESIAN_POINT ( 'NONE',  ( 1.149999999999999911, 6.472933199251450276, 6.846017351831609865 ) ) ;
#3931 = DIRECTION ( 'NONE',  ( 1.000000000000000000, 0.000000000000000000, 0.000000000000000000 ) ) ;
#3932 = CARTESIAN_POINT ( 'NONE',  ( 0.7785957873161482024, -1.940253771513320125, 2.162894899107371316 ) ) ;
#3933 = LINE ( 'NONE', #15440, #5529 ) ;
#3934 = CARTESIAN_POINT ( 'NONE',  ( 1.800000000000000044, 11.40000000000000036, 6.599999999999999645 ) ) ;
#3935 = CARTESIAN_POINT ( 'NONE',  ( 2.051331987628511211, -5.373093220338980736, 4.618035453557344461 ) ) ;
#3936 = ORIENTED_EDGE ( 'NONE', *, *, #6066, .T. ) ;
#3937 = EDGE_CURVE ( 'NONE', #9952, #7556, #7968, .T. ) ;
#3938 = LINE ( 'NONE', #13587, #3863 ) ;
#3939 = CARTESIAN_POINT ( 'NONE',  ( 1.925796468768800063, -5.404237288135590234, 6.052706598917719560 ) ) ;
#3940 = DIRECTION ( 'NONE',  ( 0.000000000000000000, -1.000000000000000000, 0.000000000000000000 ) ) ;
#3941 = ADVANCED_FACE ( 'NONE', ( #17834 ), #13614, .T. ) ;
#3942 = ORIENTED_EDGE ( 'NONE', *, *, #4825, .F. ) ;
#3943 = CARTESIAN_POINT ( 'NONE',  ( 2.224278379903029901, -5.390889830508481140, 5.468825643806100700 ) ) ;
#3944 = VECTOR ( 'NONE', #15120, 1000.000000000000000 ) ;
#3945 = ADVANCED_FACE ( 'NONE', ( #16739 ), #6749, .T. ) ;
#3946 = CARTESIAN_POINT ( 'NONE',  ( 2.349129089426440054, -0.7059744922340409623, 4.842612091679070474 ) ) ;
#3947 = CARTESIAN_POINT ( 'NONE',  ( 1.945845091385960401, -3.939205687946139900, 2.895339208235789830 ) ) ;
#3948 = VECTOR ( 'NONE', #8945, 1000.000000000000000 ) ;
#3949 = CARTESIAN_POINT ( 'NONE',  ( 0.3042893218813439438, 6.450000000000000178, 2.170710678118660031 ) ) ;
#3950 = CARTESIAN_POINT ( 'NONE',  ( 1.772995665808909660, -0.8224159336754829353, 5.735078843205156041 ) ) ;
#3951 = EDGE_CURVE ( 'NONE', #9752, #6669, #3964, .T. ) ;
#3952 = FACE_OUTER_BOUND ( 'NONE', #15929, .T. ) ;
#3953 = DIRECTION ( 'NONE',  ( 0.000000000000000000, 1.000000000000000000, 2.775557561562890365E-16 ) ) ;
#3954 = ORIENTED_EDGE ( 'NONE', *, *, #3172, .F. ) ;
#3955 = CARTESIAN_POINT ( 'NONE',  ( 1.755774834792110051, -5.260597430386769524, 2.944225165207890349 ) ) ;
#3956 = VECTOR ( 'NONE', #371, 1000.000000000000000 ) ;
#3957 = CARTESIAN_POINT ( 'NONE',  ( 0.08231150243515643339, -0.3014830508474583004, 2.050000000000001155 ) ) ;
#3958 = CARTESIAN_POINT ( 'NONE',  ( -1.507201387235980183, -3.124115597856050197, 6.507509243627219497 ) ) ;
#3959 = DIRECTION ( 'NONE',  ( -1.000000000000000000, 0.000000000000000000, 0.000000000000000000 ) ) ;
#3960 = DIRECTION ( 'NONE',  ( 1.000000000000000000, 0.000000000000000000, 0.000000000000000000 ) ) ;
#3961 = CARTESIAN_POINT ( 'NONE',  ( 1.254903241568450900, -5.426483050847465073, 7.038391080368498365 ) ) ;
#3962 = ORIENTED_EDGE ( 'NONE', *, *, #13676, .F. ) ;
#3963 = ORIENTED_EDGE ( 'NONE', *, *, #7236, .F. ) ;
#3964 = LINE ( 'NONE', #15277, #1660 ) ;
#3965 = CARTESIAN_POINT ( 'NONE',  ( -0.008736317425859809610, -0.5884632335339400333, 2.411138844410809501 ) ) ;
#3966 = EDGE_CURVE ( 'NONE', #15121, #15079, #12218, .T. ) ;
#3967 = ORIENTED_EDGE ( 'NONE', *, *, #10369, .F. ) ;
#3968 = CARTESIAN_POINT ( 'NONE',  ( 1.571912189623089873, -4.335106588847041031, 6.451524409078630562 ) ) ;
#3969 = DIRECTION ( 'NONE',  ( -4.177994306516050823E-17, 0.7310552682428690385, -0.6823182503600111470 ) ) ;
#3970 = DIRECTION ( 'NONE',  ( -1.257750167763089819E-32, 7.930164461608259947E-17, -1.000000000000000000 ) ) ;
#3971 = VECTOR ( 'NONE', #13530, 1000.000000000000000 ) ;
#3972 = CARTESIAN_POINT ( 'NONE',  ( -1.875000000000000000, 0.7500000000000000000, 8.300000000000000711 ) ) ;
#3973 = CARTESIAN_POINT ( 'NONE',  ( 1.962536940652990003, -2.704926408666860294, 5.998920491814760503 ) ) ;
#3974 = DIRECTION ( 'NONE',  ( 0.000000000000000000, 0.000000000000000000, 1.000000000000000000 ) ) ;
#3975 = CARTESIAN_POINT ( 'NONE',  ( -1.798783563193318891, -3.217268751009201289, 5.689585537188996511 ) ) ;
#3976 = ADVANCED_FACE ( 'NONE', ( #5274 ), #10822, .T. ) ;
#3977 = CARTESIAN_POINT ( 'NONE',  ( 0.02999999999999850009, 12.00000000000000000, 1.600000000000000089 ) ) ;
#3978 = CARTESIAN_POINT ( 'NONE',  ( -0.8147348917079840769, -0.2831443699174389650, 2.488757019513870183 ) ) ;
#3979 = ORIENTED_EDGE ( 'NONE', *, *, #4492, .F. ) ;
#3980 = CARTESIAN_POINT ( 'NONE',  ( -0.4735094604798580353, -4.567989471729919870, 7.005327412390699671 ) ) ;
#3981 = ORIENTED_EDGE ( 'NONE', *, *, #9111, .T. ) ;
#3982 = ORIENTED_EDGE ( 'NONE', *, *, #10149, .T. ) ;
#3983 = UNCERTAINTY_MEASURE_WITH_UNIT (LENGTH_MEASURE( 1.000000000000000082E-05 ), #14596, 'distance_accuracy_value', 'NONE');
#3984 = ADVANCED_FACE ( 'NONE', ( #11094 ), #3783, .T. ) ;
#3985 = VERTEX_POINT ( 'NONE', #15105 ) ;
#3986 = CARTESIAN_POINT ( 'NONE',  ( -1.255262969126041037E-16, 2.550000000000000266, 5.100000000000000533 ) ) ;
#3987 = CARTESIAN_POINT ( 'NONE',  ( 0.4339619423229844619, -5.139830508474575232, 6.706578715862737461 ) ) ;
#3988 = DIRECTION ( 'NONE',  ( -1.000000000000000000, -3.700743415417190112E-16, 0.000000000000000000 ) ) ;
#3989 = CARTESIAN_POINT ( 'NONE',  ( -0.5999999999999999778, 11.40000000000000036, 7.700000000000000178 ) ) ;
#3990 = DIRECTION ( 'NONE',  ( 1.000000000000000000, 0.000000000000000000, 0.000000000000000000 ) ) ;
#3991 = ADVANCED_FACE ( 'NONE', ( #1197 ), #2417, .F. ) ;
#3992 = CARTESIAN_POINT ( 'NONE',  ( -1.000000000000000000, -7.000000000000000000, 3.700000000000000178 ) ) ;
#3993 = CARTESIAN_POINT ( 'NONE',  ( -1.458615186838411626, -5.103620102360555855, 3.259477383973569786 ) ) ;
#3994 = CARTESIAN_POINT ( 'NONE',  ( -1.873832970144350130, -0.2625000000000002331, 2.826167029855650270 ) ) ;
#3995 = EDGE_LOOP ( 'NONE', ( #12271, #17307, #13480, #15399 ) ) ;
#3996 = CARTESIAN_POINT ( 'NONE',  ( 1.978267656359410154, -0.4023305084745769644, 5.974740860598790171 ) ) ;
#3997 = ORIENTED_EDGE ( 'NONE', *, *, #6717, .T. ) ;
#3998 = CARTESIAN_POINT ( 'NONE',  ( 1.554165089654128584, -0.1201271186440679706, 6.851145244874527584 ) ) ;
#3999 = DIRECTION ( 'NONE',  ( 1.836970198721028208E-16, -6.938893903907222067E-15, 1.000000000000000000 ) ) ;
#4000 = ORIENTED_EDGE ( 'NONE', *, *, #16070, .F. ) ;
#4001 = FACE_OUTER_BOUND ( 'NONE', #7063, .T. ) ;
#4002 = CARTESIAN_POINT ( 'NONE',  ( -1.167621112247339887, -2.778632149891699932, 6.743381174846779125 ) ) ;
#4003 = DIRECTION ( 'NONE',  ( 1.000000000000000000, 0.000000000000000000, 0.000000000000000000 ) ) ;
#4004 = CARTESIAN_POINT ( 'NONE',  ( 2.416676968769261080, -5.395338983050850246, 5.796598111919825769 ) ) ;
#4005 = AXIS2_PLACEMENT_3D ( 'NONE', #6605, #10972, #3728 ) ;
#4006 = CARTESIAN_POINT ( 'NONE',  ( -1.155768864438580179, -1.195028546288090743, 7.088998121597467339 ) ) ;
#4007 = ORIENTED_EDGE ( 'NONE', *, *, #4183, .T. ) ;
#4008 = CARTESIAN_POINT ( 'NONE',  ( 1.794646911016580137, -1.167899381639829981, 6.222494056560660347 ) ) ;
#4009 = CARTESIAN_POINT ( 'NONE',  ( -2.291237445532080308, -4.664983501243040287, 4.162434510291849854 ) ) ;
#4010 = EDGE_CURVE ( 'NONE', #12747, #12720, #8752, .T. ) ;
#4011 = CARTESIAN_POINT ( 'NONE',  ( 1.889999999999999902, 4.700000000000000178, 0.5999999999999999778 ) ) ;
#4012 = FACE_OUTER_BOUND ( 'NONE', #5869, .T. ) ;
#4013 = CARTESIAN_POINT ( 'NONE',  ( -1.966895454505930729, -1.703530012270459970, 5.288408118292069915 ) ) ;
#4014 = PRODUCT_DEFINITION_SHAPE ( 'NONE', 'NONE',  #2227 ) ;
#4015 = AXIS2_PLACEMENT_3D ( 'NONE', #13706, #6653, #6846 ) ;
#4016 = ORIENTED_EDGE ( 'NONE', *, *, #15036, .F. ) ;
#4017 = DIRECTION ( 'NONE',  ( -1.000000000000000000, 0.000000000000000000, 0.000000000000000000 ) ) ;
#4018 = CARTESIAN_POINT ( 'NONE',  ( 0.2000000000000000111, 0.1000000000000000056, 8.300000000000000711 ) ) ;
#4019 = CARTESIAN_POINT ( 'NONE',  ( -1.782460458101500889, -0.2002118644067801267, 5.718585207845990226 ) ) ;
#4020 = CARTESIAN_POINT ( 'NONE',  ( -1.853635285637788899, -4.408812330071866015, 6.599249831075526984 ) ) ;
#4021 = ADVANCED_FACE ( 'NONE', ( #16573 ), #13781, .F. ) ;
#4022 = AXIS2_PLACEMENT_3D ( 'NONE', #17205, #4527, #14454 ) ;
#4023 = CARTESIAN_POINT ( 'NONE',  ( -1.652654650382400003, -4.804713230972780025, 3.029252778805629820 ) ) ;
#4024 = CARTESIAN_POINT ( 'NONE',  ( -1.754713504580578842, -5.251059322033895249, 3.634325740584633646 ) ) ;
#4025 = ORIENTED_EDGE ( 'NONE', *, *, #6195, .T. ) ;
#4026 = CARTESIAN_POINT ( 'NONE',  ( 0.07299321914061039640, -0.001483050847457899725, 2.350000000000000089 ) ) ;
#4027 = DIRECTION ( 'NONE',  ( -2.220446049250309876E-16, -1.000000000000000000, -3.286920438420880041E-31 ) ) ;
#4028 = LINE ( 'NONE', #991, #4914 ) ;
#4029 = ORIENTED_EDGE ( 'NONE', *, *, #13500, .T. ) ;
#4030 =( BOUNDED_SURFACE ( )  B_SPLINE_SURFACE ( 3, 3, ( 
 ( #2354, #17424, #4744, #13450, #10394, #17584, #16134, #14746, #16228, #9184, #14846, #1233, #16875, #13649, #6596, #12523, #16511, #18136, #4094, #3825, #1051, #8810, #16959, #4268, #5852, #118, #11408, #10026, #7593, #12142, #16208, #7507, #4803, #9160, #5094, #2603, #9726, #3800, #10938, #6857, #13976, #2332, #9817, #10095, #7309, #13047, #367, #12956, #13222, #11649, #3491, #6268, #5265, #2669, #11086, #2308, #11275, #5803, #10073, #2848, #325, #11603 ),
 ( #15785, #6987, #4391, #14111, #2926, #15703, #8738, #7098, #12737, #3012, #5701, #14216, #7362, #11345, #16980, #3183, #17232, #4292, #4551, #137, #10205, #15873, #8836, #5608, #9864, #15523, #7184, #12634, #12824, #11427, #16321, #13356, #13448, #13172, #10310, #7712, #6226, #17685, #16226, #762, #15974, #2058, #489, #11800, #3354, #6395, #670, #12064, #17582, #11885, #6308, #8996, #6136, #17422, #14646, #3278, #8919, #5021, #14567, #2159, #1880, #10676 ),
 ( #11968, #13091, #9082, #7800, #13266, #3534, #409, #1807, #4915, #3626, #1959, #9276, #7450, #6048, #4742, #11694, #10571, #4826, #17322, #4652, #10476, #7528, #10392, #17505, #7618, #14744, #16132, #16056, #587, #3432, #9181, #14844, #10958, #2526, #6687, #11038, #5114, #8001, #1142, #13917, #1048, #2247, #13732, #16508, #15316, #6876, #13547, #3715, #5484, #6787, #1230, #10863, #11126, #13647, #17870, #9368, #9472, #12435, #15220, #8276, #2625, #3994 ),
 ( #13819, #18134, #14937, #8173, #4090, #16686, #15133, #7897, #10767, #18054, #16410, #12248, #5209, #16606, #3823, #12521, #2445, #8091, #9561, #16778, #5398, #864, #12344, #15042, #17965, #5311, #9648, #2352, #958, #3906, #6594, #6505, #12164, #17780, #8448, #5940, #12888, #14082, #3072, #2901, #14360, #11406, #8716, #2718, #8363, #18234, #12611, #2995, #13997, #11322, #11579, #8635, #1684, #2804, #5584, #14280, #14195, #7335, #5851, #12980, #11228, #1603 ),
 ( #1513, #16873, #204, #6962, #301, #7247, #9749, #1315, #4181, #9840, #11499, #15414, #16958, #4455, #17210, #15587, #4266, #15494, #8548, #10113, #1413, #7074, #12716, #33, #7166, #5678, #9927, #12804, #5764, #9158, #565, #14821, #3152, #13067, #11776, #6992, #8302, #5426, #2380, #980, #11063, #4208, #5612, #12461, #2546, #15345, #4019, #5234, #12640, #8201, #12274, #6716, #9674, #13940, #18078, #16806, #10889, #13751, #6901, #18266, #2651, #16539 ),
 ( #8114, #8390, #1071, #11256, #12371, #1168, #1256, #5339, #12551, #3847, #16631, #9501, #17993, #14026, #18160, #13848, #16900, #5508, #9868, #4118, #9776, #140, #14385, #14304, #7269, #12912, #17236, #5788, #10210, #15527, #5882, #7454, #58, #13094, #11430, #7102, #4475, #14117, #12742, #5704, #16135, #17689, #7715, #7622, #17782, #13358, #6310, #9371, #12252, #8367, #6689, #9564, #13822, #11581, #5587, #4270, #5766, #14284, #12890, #9163, #13337, #11948 ),
 ( #14823, #10657, #7780, #15293, #1030, #12504, #10746, #6667, #7051, #5742, #8618, #14261, #180, #11477, #7312, #6006, #7490, #3495, #13138, #15924, #10436, #4877, #10523, #14610, #11750, #7573, #2015, #4980, #14802, #2112, #4600, #11844, #17466, #4701, #3394, #9038, #15832, #3131, #2312, #3678, #8057, #12301, #13699, #1010, #9234, #14897, #13607, #7962, #6646, #16373, #2410, #17745, #1096, #7853, #16653, #9525, #10635, #2209, #13504, #822, #10921, #16284 ) ),
 .UNSPECIFIED., .T., .F., .F. ) 
 B_SPLINE_SURFACE_WITH_KNOTS ( ( 4, 3, 4 ),
 ( 4, 1, 1, 1, 1, 1, 1, 1, 1, 1, 1, 1, 1, 1, 1, 1, 1, 1, 1, 1, 1, 1, 1, 1, 1, 1, 1, 1, 1, 1, 1, 1, 1, 1, 1, 1, 1, 1, 1, 1, 1, 1, 1, 1, 1, 1, 1, 1, 1, 1, 1, 1, 1, 1, 1, 1, 1, 1, 1, 4 ),
 ( 0.000000000000000000, 3.141592653589790007, 6.283185307179590673 ),
 ( 0.000000000000000000, 0.09318283294545999518, 0.1863656658909199904, 0.2795484988363799994, 0.3727313317818399807, 0.4659141647273000175, 0.5590969976727599988, 0.6522798306182200356, 0.7454626635636799614, 0.8386454965091399982, 0.9318283294545990358, 1.025011162400059961, 1.118193995345519998, 1.211376828290979812, 1.304559661236440071, 1.397742494181900108, 1.490925327127359923, 1.584108160072819960, 1.677290993018279996, 1.770473825963740033, 1.863656658909200070, 1.956839491854659885, 2.050022324800119922, 2.143205157745580181, 2.236387990691039995, 2.329570823636499810, 2.422753656581960069, 2.515936489527420328, 2.609119322472880143, 2.702302155418339957, 2.795484988363799772, 2.888667821309260031, 2.981850654254720290, 3.075033487200180105, 3.168216320145639919, 3.261399153091099734, 3.354581986036559993, 3.447764818982019808, 3.540947651927480067, 3.634130484872939881, 3.727313317818400140, 3.820496150763859955, 3.913678983709319770, 4.006861816654780029, 4.100044649600239843, 4.193227482545699658, 4.286410315491160361, 4.379593148436620176, 4.472775981382079991, 4.565958814327539805, 4.659141647272999620, 4.752324480218450553, 4.845507313163910368, 4.938690146109370183, 5.031872979054829997, 5.125055812000289812, 5.218238644945749627, 5.311421477891210330, 5.404604310836670145, 5.497787143782139729 ),
 .UNSPECIFIED. ) 
 GEOMETRIC_REPRESENTATION_ITEM ( )  RATIONAL_B_SPLINE_SURFACE ( (
 ( 1.000000000000000000, 1.000000000000000000, 1.000000000000000000, 1.000000000000000000, 1.000000000000000000, 1.000000000000000000, 1.000000000000000000, 1.000000000000000000, 1.000000000000000000, 1.000000000000000000, 1.000000000000000000, 1.000000000000000000, 1.000000000000000000, 1.000000000000000000, 1.000000000000000000, 1.000000000000000000, 1.000000000000000000, 1.000000000000000000, 1.000000000000000000, 1.000000000000000000, 1.000000000000000000, 1.000000000000000000, 1.000000000000000000, 1.000000000000000000, 1.000000000000000000, 1.000000000000000000, 1.000000000000000000, 1.000000000000000000, 1.000000000000000000, 1.000000000000000000, 1.000000000000000000, 1.000000000000000000, 1.000000000000000000, 1.000000000000000000, 1.000000000000000000, 1.000000000000000000, 1.000000000000000000, 1.000000000000000000, 1.000000000000000000, 1.000000000000000000, 1.000000000000000000, 1.000000000000000000, 1.000000000000000000, 1.000000000000000000, 1.000000000000000000, 1.000000000000000000, 1.000000000000000000, 1.000000000000000000, 1.000000000000000000, 1.000000000000000000, 1.000000000000000000, 1.000000000000000000, 1.000000000000000000, 1.000000000000000000, 1.000000000000000000, 1.000000000000000000, 1.000000000000000000, 1.000000000000000000, 1.000000000000000000, 1.000000000000000000, 1.000000000000000000, 1.000000000000000000),
 ( 0.3333333333333329818, 0.3333333333333329818, 0.3333333333333329818, 0.3333333333333329818, 0.3333333333333329818, 0.3333333333333329818, 0.3333333333333329818, 0.3333333333333329818, 0.3333333333333329818, 0.3333333333333329818, 0.3333333333333329818, 0.3333333333333329818, 0.3333333333333329818, 0.3333333333333329818, 0.3333333333333329818, 0.3333333333333329818, 0.3333333333333329818, 0.3333333333333329818, 0.3333333333333329818, 0.3333333333333329818, 0.3333333333333329818, 0.3333333333333329818, 0.3333333333333329818, 0.3333333333333329818, 0.3333333333333329818, 0.3333333333333329818, 0.3333333333333329818, 0.3333333333333329818, 0.3333333333333329818, 0.3333333333333329818, 0.3333333333333329818, 0.3333333333333329818, 0.3333333333333329818, 0.3333333333333329818, 0.3333333333333329818, 0.3333333333333329818, 0.3333333333333329818, 0.3333333333333329818, 0.3333333333333329818, 0.3333333333333329818, 0.3333333333333329818, 0.3333333333333329818, 0.3333333333333329818, 0.3333333333333329818, 0.3333333333333329818, 0.3333333333333329818, 0.3333333333333329818, 0.3333333333333329818, 0.3333333333333329818, 0.3333333333333329818, 0.3333333333333329818, 0.3333333333333329818, 0.3333333333333329818, 0.3333333333333329818, 0.3333333333333329818, 0.3333333333333329818, 0.3333333333333329818, 0.3333333333333329818, 0.3333333333333329818, 0.3333333333333329818, 0.3333333333333329818, 0.3333333333333329818),
 ( 0.3333333333333329818, 0.3333333333333329818, 0.3333333333333329818, 0.3333333333333329818, 0.3333333333333329818, 0.3333333333333329818, 0.3333333333333329818, 0.3333333333333329818, 0.3333333333333329818, 0.3333333333333329818, 0.3333333333333329818, 0.3333333333333329818, 0.3333333333333329818, 0.3333333333333329818, 0.3333333333333329818, 0.3333333333333329818, 0.3333333333333329818, 0.3333333333333329818, 0.3333333333333329818, 0.3333333333333329818, 0.3333333333333329818, 0.3333333333333329818, 0.3333333333333329818, 0.3333333333333329818, 0.3333333333333329818, 0.3333333333333329818, 0.3333333333333329818, 0.3333333333333329818, 0.3333333333333329818, 0.3333333333333329818, 0.3333333333333329818, 0.3333333333333329818, 0.3333333333333329818, 0.3333333333333329818, 0.3333333333333329818, 0.3333333333333329818, 0.3333333333333329818, 0.3333333333333329818, 0.3333333333333329818, 0.3333333333333329818, 0.3333333333333329818, 0.3333333333333329818, 0.3333333333333329818, 0.3333333333333329818, 0.3333333333333329818, 0.3333333333333329818, 0.3333333333333329818, 0.3333333333333329818, 0.3333333333333329818, 0.3333333333333329818, 0.3333333333333329818, 0.3333333333333329818, 0.3333333333333329818, 0.3333333333333329818, 0.3333333333333329818, 0.3333333333333329818, 0.3333333333333329818, 0.3333333333333329818, 0.3333333333333329818, 0.3333333333333329818, 0.3333333333333329818, 0.3333333333333329818),
 ( 1.000000000000000000, 1.000000000000000000, 1.000000000000000000, 1.000000000000000000, 1.000000000000000000, 1.000000000000000000, 1.000000000000000000, 1.000000000000000000, 1.000000000000000000, 1.000000000000000000, 1.000000000000000000, 1.000000000000000000, 1.000000000000000000, 1.000000000000000000, 1.000000000000000000, 1.000000000000000000, 1.000000000000000000, 1.000000000000000000, 1.000000000000000000, 1.000000000000000000, 1.000000000000000000, 1.000000000000000000, 1.000000000000000000, 1.000000000000000000, 1.000000000000000000, 1.000000000000000000, 1.000000000000000000, 1.000000000000000000, 1.000000000000000000, 1.000000000000000000, 1.000000000000000000, 1.000000000000000000, 1.000000000000000000, 1.000000000000000000, 1.000000000000000000, 1.000000000000000000, 1.000000000000000000, 1.000000000000000000, 1.000000000000000000, 1.000000000000000000, 1.000000000000000000, 1.000000000000000000, 1.000000000000000000, 1.000000000000000000, 1.000000000000000000, 1.000000000000000000, 1.000000000000000000, 1.000000000000000000, 1.000000000000000000, 1.000000000000000000, 1.000000000000000000, 1.000000000000000000, 1.000000000000000000, 1.000000000000000000, 1.000000000000000000, 1.000000000000000000, 1.000000000000000000, 1.000000000000000000, 1.000000000000000000, 1.000000000000000000, 1.000000000000000000, 1.000000000000000000),
 ( 0.3333333333333329818, 0.3333333333333329818, 0.3333333333333329818, 0.3333333333333329818, 0.3333333333333329818, 0.3333333333333329818, 0.3333333333333329818, 0.3333333333333329818, 0.3333333333333329818, 0.3333333333333329818, 0.3333333333333329818, 0.3333333333333329818, 0.3333333333333329818, 0.3333333333333329818, 0.3333333333333329818, 0.3333333333333329818, 0.3333333333333329818, 0.3333333333333329818, 0.3333333333333329818, 0.3333333333333329818, 0.3333333333333329818, 0.3333333333333329818, 0.3333333333333329818, 0.3333333333333329818, 0.3333333333333329818, 0.3333333333333329818, 0.3333333333333329818, 0.3333333333333329818, 0.3333333333333329818, 0.3333333333333329818, 0.3333333333333329818, 0.3333333333333329818, 0.3333333333333329818, 0.3333333333333329818, 0.3333333333333329818, 0.3333333333333329818, 0.3333333333333329818, 0.3333333333333329818, 0.3333333333333329818, 0.3333333333333329818, 0.3333333333333329818, 0.3333333333333329818, 0.3333333333333329818, 0.3333333333333329818, 0.3333333333333329818, 0.3333333333333329818, 0.3333333333333329818, 0.3333333333333329818, 0.3333333333333329818, 0.3333333333333329818, 0.3333333333333329818, 0.3333333333333329818, 0.3333333333333329818, 0.3333333333333329818, 0.3333333333333329818, 0.3333333333333329818, 0.3333333333333329818, 0.3333333333333329818, 0.3333333333333329818, 0.3333333333333329818, 0.3333333333333329818, 0.3333333333333329818),
 ( 0.3333333333333329818, 0.3333333333333329818, 0.3333333333333329818, 0.3333333333333329818, 0.3333333333333329818, 0.3333333333333329818, 0.3333333333333329818, 0.3333333333333329818, 0.3333333333333329818, 0.3333333333333329818, 0.3333333333333329818, 0.3333333333333329818, 0.3333333333333329818, 0.3333333333333329818, 0.3333333333333329818, 0.3333333333333329818, 0.3333333333333329818, 0.3333333333333329818, 0.3333333333333329818, 0.3333333333333329818, 0.3333333333333329818, 0.3333333333333329818, 0.3333333333333329818, 0.3333333333333329818, 0.3333333333333329818, 0.3333333333333329818, 0.3333333333333329818, 0.3333333333333329818, 0.3333333333333329818, 0.3333333333333329818, 0.3333333333333329818, 0.3333333333333329818, 0.3333333333333329818, 0.3333333333333329818, 0.3333333333333329818, 0.3333333333333329818, 0.3333333333333329818, 0.3333333333333329818, 0.3333333333333329818, 0.3333333333333329818, 0.3333333333333329818, 0.3333333333333329818, 0.3333333333333329818, 0.3333333333333329818, 0.3333333333333329818, 0.3333333333333329818, 0.3333333333333329818, 0.3333333333333329818, 0.3333333333333329818, 0.3333333333333329818, 0.3333333333333329818, 0.3333333333333329818, 0.3333333333333329818, 0.3333333333333329818, 0.3333333333333329818, 0.3333333333333329818, 0.3333333333333329818, 0.3333333333333329818, 0.3333333333333329818, 0.3333333333333329818, 0.3333333333333329818, 0.3333333333333329818),
 ( 1.000000000000000000, 1.000000000000000000, 1.000000000000000000, 1.000000000000000000, 1.000000000000000000, 1.000000000000000000, 1.000000000000000000, 1.000000000000000000, 1.000000000000000000, 1.000000000000000000, 1.000000000000000000, 1.000000000000000000, 1.000000000000000000, 1.000000000000000000, 1.000000000000000000, 1.000000000000000000, 1.000000000000000000, 1.000000000000000000, 1.000000000000000000, 1.000000000000000000, 1.000000000000000000, 1.000000000000000000, 1.000000000000000000, 1.000000000000000000, 1.000000000000000000, 1.000000000000000000, 1.000000000000000000, 1.000000000000000000, 1.000000000000000000, 1.000000000000000000, 1.000000000000000000, 1.000000000000000000, 1.000000000000000000, 1.000000000000000000, 1.000000000000000000, 1.000000000000000000, 1.000000000000000000, 1.000000000000000000, 1.000000000000000000, 1.000000000000000000, 1.000000000000000000, 1.000000000000000000, 1.000000000000000000, 1.000000000000000000, 1.000000000000000000, 1.000000000000000000, 1.000000000000000000, 1.000000000000000000, 1.000000000000000000, 1.000000000000000000, 1.000000000000000000, 1.000000000000000000, 1.000000000000000000, 1.000000000000000000, 1.000000000000000000, 1.000000000000000000, 1.000000000000000000, 1.000000000000000000, 1.000000000000000000, 1.000000000000000000, 1.000000000000000000, 1.000000000000000000) ) ) 
 REPRESENTATION_ITEM ( '' )  SURFACE ( )  );
#4031 = CARTESIAN_POINT ( 'NONE',  ( -1.750316316486840051, -5.559957627118639500, 3.126818518378589928 ) ) ;
#4032 = CARTESIAN_POINT ( 'NONE',  ( 2.065623031241559548, -0.5662447625043109944, 3.572193642975259653 ) ) ;
#4033 = VECTOR ( 'NONE', #6680, 1000.000000000000000 ) ;
#4034 = VECTOR ( 'NONE', #4386, 1000.000000000000000 ) ;
#4035 = LINE ( 'NONE', #2662, #5558 ) ;
#4036 = CARTESIAN_POINT ( 'NONE',  ( -2.053018524985070314, -1.474488005747551567, 4.695903819313384631 ) ) ;
#4037 = DIRECTION ( 'NONE',  ( -6.123233995736779594E-17, -2.493473113004680074E-16, -1.000000000000000000 ) ) ;
#4038 = EDGE_CURVE ( 'NONE', #389, #4246, #16736, .T. ) ;
#4039 = ORIENTED_EDGE ( 'NONE', *, *, #1671, .T. ) ;
#4040 = ADVANCED_FACE ( 'NONE', ( #5370 ), #13881, .F. ) ;
#4041 = AXIS2_PLACEMENT_3D ( 'NONE', #12558, #1265, #14227 ) ;
#4042 = ADVANCED_FACE ( 'NONE', ( #9919 ), #1226, .T. ) ;
#4043 = CARTESIAN_POINT ( 'NONE',  ( 1.000000000000002220, 9.099999999999999645, 8.300000000000000711 ) ) ;
#4044 = CARTESIAN_POINT ( 'NONE',  ( 1.973760952634081134, -0.3400423728813561364, 2.925986839873718992 ) ) ;
#4045 = EDGE_CURVE ( 'NONE', #8261, #7811, #18187, .T. ) ;
#4046 = CARTESIAN_POINT ( 'NONE',  ( 1.832842064134690085, -2.728214696955149954, 6.176291182464479945 ) ) ;
#4047 = CARTESIAN_POINT ( 'NONE',  ( -1.899999999999999911, 0.7211102550927980248, 7.649999999999999467 ) ) ;
#4048 = DIRECTION ( 'NONE',  ( 1.000000000000000000, 1.283953296258166085E-32, -6.123233995736769734E-17 ) ) ;
#4049 = CARTESIAN_POINT ( 'NONE',  ( -1.192209327851089240, -5.577754237288145234, 2.329031440774910422 ) ) ;
#4050 = ORIENTED_EDGE ( 'NONE', *, *, #13543, .F. ) ;
#4051 = VECTOR ( 'NONE', #1810, 1000.000000000000000 ) ;
#4052 = LINE ( 'NONE', #4422, #7137 ) ;
#4053 = CARTESIAN_POINT ( 'NONE',  ( 1.889999999999999902, 7.299999999999999822, 0.6099999999999999867 ) ) ;
#4054 = LINE ( 'NONE', #3685, #544 ) ;
#4055 = VECTOR ( 'NONE', #15159, 1000.000000000000000 ) ;
#4056 = ORIENTED_EDGE ( 'NONE', *, *, #7413, .F. ) ;
#4057 = VECTOR ( 'NONE', #15488, 1000.000000000000000 ) ;
#4058 = CARTESIAN_POINT ( 'NONE',  ( -1.626408692231610109, -4.707719201459649838, 6.401040991074980369 ) ) ;
#4059 = CARTESIAN_POINT ( 'NONE',  ( 1.147638118088980086, -5.328211948015596278, 2.987995008461610702 ) ) ;
#4060 = CARTESIAN_POINT ( 'NONE',  ( 1.899999999999999911, 11.40000000000000036, 6.599999999999999645 ) ) ;
#4061 = CARTESIAN_POINT ( 'NONE',  ( -1.250000000000000000, 3.500000000000000000, 5.100000000000000533 ) ) ;
#4062 = AXIS2_PLACEMENT_3D ( 'NONE', #11448, #506, #1638 ) ;
#4063 = CARTESIAN_POINT ( 'NONE',  ( 2.342931736853870017, -4.102223705964150646, 4.477701633099130163 ) ) ;
#4064 = AXIS2_PLACEMENT_3D ( 'NONE', #7464, #6153, #3105 ) ;
#4065 = FACE_OUTER_BOUND ( 'NONE', #2435, .T. ) ;
#4066 = CARTESIAN_POINT ( 'NONE',  ( -1.160665242129840014, -3.100827309567759205, 6.393445611273007145 ) ) ;
#4067 = ADVANCED_FACE ( 'NONE', ( #5480 ), #8630, .F. ) ;
#4068 = CARTESIAN_POINT ( 'NONE',  ( 4.898587196589409994E-17, 0.1000000000000000056, 8.300000000000000711 ) ) ;
#4069 = AXIS2_PLACEMENT_3D ( 'NONE', #12224, #12136, #14814 ) ;
#4070 = ORIENTED_EDGE ( 'NONE', *, *, #216, .F. ) ;
#4071 = CARTESIAN_POINT ( 'NONE',  ( -1.221947981261169991, -0.5741044150835520332, 2.670403636935529956 ) ) ;
#4072 = ORIENTED_EDGE ( 'NONE', *, *, #10168, .T. ) ;
#4073 = AXIS2_PLACEMENT_3D ( 'NONE', #17465, #7572, #17546 ) ;
#4074 = DIRECTION ( 'NONE',  ( 1.000000000000000000, 0.000000000000000000, 0.000000000000000000 ) ) ;
#4075 = LINE ( 'NONE', #3807, #11646 ) ;
#4076 = ORIENTED_EDGE ( 'NONE', *, *, #10243, .F. ) ;
#4077 = EDGE_LOOP ( 'NONE', ( #11234, #7732, #14892, #17804 ) ) ;
#4078 = VECTOR ( 'NONE', #13750, 1000.000000000000000 ) ;
#4079 = ORIENTED_EDGE ( 'NONE', *, *, #2944, .T. ) ;
#4080 = CARTESIAN_POINT ( 'NONE',  ( -1.875000000000000000, 2.296212748401290437E-16, 8.300000000000000711 ) ) ;
#4081 = CARTESIAN_POINT ( 'NONE',  ( -0.2189795514005259958, -5.295550847457629828, 2.356806637999020015 ) ) ;
#4082 = FACE_OUTER_BOUND ( 'NONE', #1351, .T. ) ;
#4083 = LINE ( 'NONE', #11399, #802 ) ;
#4084 = VECTOR ( 'NONE', #9231, 1000.000000000000000 ) ;
#4085 = AXIS2_PLACEMENT_3D ( 'NONE', #4923, #871, #5212 ) ;
#4086 = LINE ( 'NONE', #15680, #13206 ) ;
#4087 = DIRECTION ( 'NONE',  ( 1.000000000000000000, -2.220446049250309876E-16, -1.048990684667790150E-15 ) ) ;
#4088 = CARTESIAN_POINT ( 'NONE',  ( -1.703239418290670049, -5.057043525783965876, 3.553755118148739900 ) ) ;
#4089 = CARTESIAN_POINT ( 'NONE',  ( -1.712910428781911021, -2.895073591333140239, 5.831741890007735130 ) ) ;
#4090 = CARTESIAN_POINT ( 'NONE',  ( 0.6493550500446280127, -0.01334745762711890028, 2.437955526623099889 ) ) ;
#4091 = EDGE_CURVE ( 'NONE', #17492, #6294, #11121, .T. ) ;
#4092 = VECTOR ( 'NONE', #15445, 1000.000000000000000 ) ;
#4093 = ORIENTED_EDGE ( 'NONE', *, *, #8846, .F. ) ;
#4094 = CARTESIAN_POINT ( 'NONE',  ( 2.353194804772640314, -0.3756355932203400139, 4.731327187377229571 ) ) ;
#4095 = CARTESIAN_POINT ( 'NONE',  ( -0.2812789908084309953, -0.4557203389830509765, 7.036533610117280624 ) ) ;
#4096 = VERTEX_POINT ( 'NONE', #4356 ) ;
#4097 = CARTESIAN_POINT ( 'NONE',  ( 1.000896394980339998, -0.1290254237288140093, 6.829956240957369751 ) ) ;
#4098 = CARTESIAN_POINT ( 'NONE',  ( 2.331386066015260106, -0.9583047870452390260, 4.378465089518139841 ) ) ;
#4099 = VERTEX_POINT ( 'NONE', #6957 ) ;
#4100 = AXIS2_PLACEMENT_3D ( 'NONE', #11217, #13807, #15486 ) ;
#4101 = VECTOR ( 'NONE', #10628, 1000.000000000000000 ) ;
#4102 = CARTESIAN_POINT ( 'NONE',  ( -1.800000000000000044, 12.00000000000000000, 7.649999999999999467 ) ) ;
#4103 = ORIENTED_EDGE ( 'NONE', *, *, #10149, .F. ) ;
#4104 = CARTESIAN_POINT ( 'NONE',  ( -2.301223891756910334, -2.988226744486290887, 5.193066210047998510 ) ) ;
#4105 = CARTESIAN_POINT ( 'NONE',  ( 2.519547246525509543, -5.359745762711870753, 3.866491354109194756 ) ) ;
#4106 = VERTEX_POINT ( 'NONE', #5579 ) ;
#4107 = CARTESIAN_POINT ( 'NONE',  ( -0.1569242594330230167, -1.400782264522720144, 7.048216443236290374 ) ) ;
#4108 = CARTESIAN_POINT ( 'NONE',  ( 1.438959988998139914E-16, -0.2999999999999999889, 2.350000000000000089 ) ) ;
#4109 = ORIENTED_EDGE ( 'NONE', *, *, #7557, .T. ) ;
#4110 = LINE ( 'NONE', #1159, #14078 ) ;
#4111 = CARTESIAN_POINT ( 'NONE',  ( 1.399999999999998579, -9.792893218813446765, 3.300000000000000266 ) ) ;
#4112 = CARTESIAN_POINT ( 'NONE',  ( -1.550000000000000044, -6.000000000000000000, 6.100000000000000533 ) ) ;
#4113 = AXIS2_PLACEMENT_3D ( 'NONE', #507, #5981, #11622 ) ;
#4114 = CARTESIAN_POINT ( 'NONE',  ( -1.903446074666951260, -1.680241723982170754, 5.469282057156605426 ) ) ;
#4115 = CARTESIAN_POINT ( 'NONE',  ( 5.204748896376257478E-17, 2.600000000000000089, 8.250000000000000000 ) ) ;
#4116 = CARTESIAN_POINT ( 'NONE',  ( -1.889999999999999902, 8.500000000000000000, 0.6099999999999999867 ) ) ;
#4117 = CARTESIAN_POINT ( 'NONE',  ( 7.347880794884119736E-16, -6.000000000000000000, -3.673940397442060361E-16 ) ) ;
#4118 = CARTESIAN_POINT ( 'NONE',  ( 2.041338374031088865, -0.3800847457627119508, 4.918217215283659627 ) ) ;
#4119 = PRODUCT_DEFINITION_FORMATION_WITH_SPECIFIED_SOURCE ( 'ANY', '', #6678, .NOT_KNOWN. ) ;
#4120 = CARTESIAN_POINT ( 'NONE',  ( 1.930452136971109622, -4.012911429170968880, 6.521117305355573102 ) ) ;
#4121 = CARTESIAN_POINT ( 'NONE',  ( -0.4068869028847361125, -5.251463457376924104, 2.679545647941359743 ) ) ;
#4122 = CARTESIAN_POINT ( 'NONE',  ( -0.3265524029357583236, -5.157627118644064979, 6.726831181542982208 ) ) ;
#4123 = ORIENTED_EDGE ( 'NONE', *, *, #17038, .T. ) ;
#4124 = EDGE_CURVE ( 'NONE', #5861, #3042, #1309, .T. ) ;
#4125 = CARTESIAN_POINT ( 'NONE',  ( 0.5500000000000000444, 3.050000000000000266, 3.399999999999999911 ) ) ;
#4126 = DIRECTION ( 'NONE',  ( 0.7071067811865470176, 4.329780281177469511E-17, -0.7071067811865480168 ) ) ;
#4127 = CIRCLE ( 'NONE', #11224, 0.01000000000000002623 ) ;
#4128 = CARTESIAN_POINT ( 'NONE',  ( -1.687197751398160861, -0.5672554343907065810, 2.639290338773708999 ) ) ;
#4129 = EDGE_LOOP ( 'NONE', ( #163, #5291, #14228, #16858 ) ) ;
#4130 = CARTESIAN_POINT ( 'NONE',  ( 2.500000000000000000, 9.199999999999999289, 1.600000000000000089 ) ) ;
#4131 = CARTESIAN_POINT ( 'NONE',  ( 2.281778813005790330, -0.7525510688106179513, 5.276394947932120161 ) ) ;
#4132 = CARTESIAN_POINT ( 'NONE',  ( 0.5500000000000000444, -2.399999999999999911, 3.600000000000000089 ) ) ;
#4133 = CARTESIAN_POINT ( 'NONE',  ( -0.5381211601353440566, -1.148451969711520082, 6.681243917250651698 ) ) ;
#4134 = CARTESIAN_POINT ( 'NONE',  ( -0.9999999999999978906, 9.099999999999999645, 8.300000000000000711 ) ) ;
#4135 = ORIENTED_EDGE ( 'NONE', *, *, #8669, .F. ) ;
#4136 = VECTOR ( 'NONE', #11187, 1000.000000000000000 ) ;
#4137 = FACE_OUTER_BOUND ( 'NONE', #10904, .T. ) ;
#4138 = CARTESIAN_POINT ( 'NONE',  ( 0.4917262214558945632, -0.3088983050847459166, 2.092115739186370948 ) ) ;
#4139 = CARTESIAN_POINT ( 'NONE',  ( -2.351999299633229956, -3.333710192450639820, 4.782734406438290620 ) ) ;
#4140 = PLANE ( 'NONE',  #14886 ) ;
#4141 = FACE_OUTER_BOUND ( 'NONE', #11507, .T. ) ;
#4142 = CARTESIAN_POINT ( 'NONE',  ( -2.601107615185130673, -5.515466101694915579, 5.226397344856384741 ) ) ;
#4143 = EDGE_LOOP ( 'NONE', ( #17872, #1980, #5813, #3893 ) ) ;
#4144 = ORIENTED_EDGE ( 'NONE', *, *, #17863, .T. ) ;
#4145 = CARTESIAN_POINT ( 'NONE',  ( -0.07299321914061848715, -5.298516949152539013, 2.350000000000000089 ) ) ;
#4146 = DIRECTION ( 'NONE',  ( 1.000000000000000000, 0.000000000000000000, 0.000000000000000000 ) ) ;
#4147 = CARTESIAN_POINT ( 'NONE',  ( 1.899999999999999911, 4.700000000000000178, 1.600000000000000089 ) ) ;
#4148 = EDGE_LOOP ( 'NONE', ( #16986, #7271, #3617, #2123, #11243, #15003, #12400, #6485 ) ) ;
#4149 = AXIS2_PLACEMENT_3D ( 'NONE', #9505, #2471, #11998 ) ;
#4150 = CARTESIAN_POINT ( 'NONE',  ( 2.343457872958619959, -4.148800282540729967, 4.916681529328559286 ) ) ;
#4151 = EDGE_CURVE ( 'NONE', #17998, #12255, #9643, .T. ) ;
#4152 = CARTESIAN_POINT ( 'NONE',  ( -0.009452110982655128821, -0.5998079552954630467, 2.350000000000000089 ) ) ;
#4153 = CARTESIAN_POINT ( 'NONE',  ( -0.2335786437626909962, 3.050000000000000266, 1.958578643762689753 ) ) ;
#4154 = ADVANCED_FACE ( 'NONE', ( #2988 ), #5393, .F. ) ;
#4155 = CARTESIAN_POINT ( 'NONE',  ( -1.550000000000000044, -5.599999999999999645, 6.100000000000000533 ) ) ;
#4156 = EDGE_CURVE ( 'NONE', #8493, #13928, #15310, .T. ) ;
#4157 = DIRECTION ( 'NONE',  ( -0.7071067811865475727, 0.000000000000000000, 0.7071067811865475727 ) ) ;
#4158 = CARTESIAN_POINT ( 'NONE',  ( -2.033393610350109793, -4.777584066324510381, 5.884928737465370041 ) ) ;
#4159 = CARTESIAN_POINT ( 'NONE',  ( 0.1749999999999999889, 7.799999999999999822, 0.4000000000000000222 ) ) ;
#4160 = CARTESIAN_POINT ( 'NONE',  ( 1.599895119336370852, -2.728214696955149510, 5.986560317183676538 ) ) ;
#4161 = FACE_OUTER_BOUND ( 'NONE', #309, .T. ) ;
#4162 = AXIS2_PLACEMENT_3D ( 'NONE', #10507, #16168, #11634 ) ;
#4163 = ORIENTED_EDGE ( 'NONE', *, *, #8017, .F. ) ;
#4164 = CARTESIAN_POINT ( 'NONE',  ( 1.899999999999999911, 7.299999999999999822, 0.5999999999999999778 ) ) ;
#4165 = ORIENTED_EDGE ( 'NONE', *, *, #8662, .T. ) ;
#4166 = ORIENTED_EDGE ( 'NONE', *, *, #2059, .T. ) ;
#4167 = ORIENTED_EDGE ( 'NONE', *, *, #11288, .T. ) ;
#4168 = ORIENTED_EDGE ( 'NONE', *, *, #3604, .T. ) ;
#4169 = CARTESIAN_POINT ( 'NONE',  ( -0.5500000000000000444, 3.050000000000000266, 3.299999999999999822 ) ) ;
#4170 = CARTESIAN_POINT ( 'NONE',  ( -0.7476103186298618253, -5.282203389830510076, 2.787995836256459636 ) ) ;
#4171 = PRODUCT_DEFINITION_SHAPE ( 'NONE', 'NONE',  #18294 ) ;
#4172 = CARTESIAN_POINT ( 'NONE',  ( 0.5385843327681005821, -1.916965483225031130, 2.101338688959521139 ) ) ;
#4173 = EDGE_CURVE ( 'NONE', #5456, #3896, #8442, .T. ) ;
#4174 = LINE ( 'NONE', #6868, #16180 ) ;
#4175 = DIRECTION ( 'NONE',  ( 0.000000000000000000, -1.000000000000000000, 0.000000000000000000 ) ) ;
#4176 = DIRECTION ( 'NONE',  ( 0.000000000000000000, 0.000000000000000000, 1.000000000000000000 ) ) ;
#4177 = CARTESIAN_POINT ( 'NONE',  ( -0.4649462444738060030, -5.251463457376920552, 2.383584851084299849 ) ) ;
#4178 = CARTESIAN_POINT ( 'NONE',  ( -1.889999999999999902, 4.100000000000000533, 0.5999999999999999778 ) ) ;
#4179 = CARTESIAN_POINT ( 'NONE',  ( -0.2023972492402590084, -2.146007489747939978, 2.355265251465770149 ) ) ;
#4180 = CARTESIAN_POINT ( 'NONE',  ( 0.08304008649498713368, -2.638902420161969520, 6.751342532748487280 ) ) ;
#4181 = CARTESIAN_POINT ( 'NONE',  ( 1.246151616534670215, -0.03114406779661053892, 3.068501529594759081 ) ) ;
#4182 = ORIENTED_EDGE ( 'NONE', *, *, #7864, .T. ) ;
#4183 = EDGE_CURVE ( 'NONE', #12988, #7791, #12710, .T. ) ;
#4184 = CARTESIAN_POINT ( 'NONE',  ( 2.088297318559229954, -0.3978813559322040283, 5.785136623276629919 ) ) ;
#4185 = LINE ( 'NONE', #3075, #10932 ) ;
#4186 = ORIENTED_EDGE ( 'NONE', *, *, #1514, .F. ) ;
#4187 = CARTESIAN_POINT ( 'NONE',  ( 2.340070819011249803, -0.08008474576271229495, 4.950151441910540129 ) ) ;
#4188 = CARTESIAN_POINT ( 'NONE',  ( -0.3752419433106839453, -1.424070552810999812, 7.023346545710370314 ) ) ;
#4189 = ORIENTED_EDGE ( 'NONE', *, *, #14908, .T. ) ;
#4190 = ORIENTED_EDGE ( 'NONE', *, *, #3751, .T. ) ;
#4191 = CARTESIAN_POINT ( 'NONE',  ( 0.8986180677147457274, -1.963542059801610229, 2.524860635301610312 ) ) ;
#4192 = CARTESIAN_POINT ( 'NONE',  ( 0.000000000000000000, 0.000000000000000000, 0.000000000000000000 ) ) ;
#4193 = CARTESIAN_POINT ( 'NONE',  ( -1.925836318347889931, -5.488771186440680516, 6.525927015348141680 ) ) ;
#4194 = EDGE_CURVE ( 'NONE', #1195, #14289, #17373, .T. ) ;
#4195 = VERTEX_POINT ( 'NONE', #2893 ) ;
#4196 = CARTESIAN_POINT ( 'NONE',  ( 1.652654650382400003, -0.7952867690272209522, 3.029252778805620050 ) ) ;
#4197 = CARTESIAN_POINT ( 'NONE',  ( -1.782460458101500889, -0.5002118644067795605, 5.718585207845990226 ) ) ;
#4198 = ORIENTED_EDGE ( 'NONE', *, *, #7643, .F. ) ;
#4199 = LINE ( 'NONE', #3840, #8181 ) ;
#4200 = LINE ( 'NONE', #9860, #3767 ) ;
#4201 = FACE_OUTER_BOUND ( 'NONE', #8507, .T. ) ;
#4202 = VECTOR ( 'NONE', #17148, 1000.000000000000000 ) ;
#4203 = CARTESIAN_POINT ( 'NONE',  ( -0.8735826871841183561, -1.493935417675870791, 6.557889967484691773 ) ) ;
#4204 = CARTESIAN_POINT ( 'NONE',  ( -2.500000000000000000, 0.7500000000000000000, 7.649999999999999467 ) ) ;
#4205 = VERTEX_POINT ( 'NONE', #8540 ) ;
#4206 = CARTESIAN_POINT ( 'NONE',  ( 1.889999999999999902, 7.900000000000000355, 3.000000000000000000 ) ) ;
#4207 = CARTESIAN_POINT ( 'NONE',  ( -0.1749999999999999889, 9.099999999999999645, 0.4000000000000000222 ) ) ;
#4208 = CARTESIAN_POINT ( 'NONE',  ( -1.134881315981510541, -0.1779661016949160846, 6.410767520434657918 ) ) ;
#4209 = CARTESIAN_POINT ( 'NONE',  ( -0.4649462444738060030, -5.251463457376920552, 2.383584851084299849 ) ) ;
#4210 = CARTESIAN_POINT ( 'NONE',  ( -1.526871680339578541, -5.259957627118655665, 3.327650196883449762 ) ) ;
#4211 = ORIENTED_EDGE ( 'NONE', *, *, #7129, .T. ) ;
#4212 = VECTOR ( 'NONE', #5424, 1000.000000000000000 ) ;
#4213 = DIRECTION ( 'NONE',  ( -0.7071067811865475727, 0.000000000000000000, 0.7071067811865475727 ) ) ;
#4214 = CARTESIAN_POINT ( 'NONE',  ( 1.899999999999999911, 4.700000000000000178, 0.6099999999999999867 ) ) ;
#4215 = DIRECTION ( 'NONE',  ( 0.000000000000000000, 1.000000000000000000, 0.000000000000000000 ) ) ;
#4216 = EDGE_CURVE ( 'NONE', #11075, #16312, #8486, .T. ) ;
#4217 = ORIENTED_EDGE ( 'NONE', *, *, #1811, .T. ) ;
#4218 = DIRECTION ( 'NONE',  ( -1.000000000000000000, 0.000000000000000000, 3.700743415417190112E-16 ) ) ;
#4219 = CARTESIAN_POINT ( 'NONE',  ( 0.4790341583531380065, -1.916965483225030242, 2.395814251711720022 ) ) ;
#4220 = CYLINDRICAL_SURFACE ( 'NONE', #3450, 0.09999999999999982514 ) ;
#4221 = CARTESIAN_POINT ( 'NONE',  ( -2.331386066015260106, -4.641695212954759953, 4.378465089518190467 ) ) ;
#4222 = CARTESIAN_POINT ( 'NONE',  ( 0.1749999999999999889, 8.800000000000000711, 0.4000000000000000222 ) ) ;
#4223 = AXIS2_PLACEMENT_3D ( 'NONE', #5537, #2954, #11185 ) ;
#4224 = ORIENTED_EDGE ( 'NONE', *, *, #16302, .F. ) ;
#4225 = CARTESIAN_POINT ( 'NONE',  ( -0.1749999999999999889, 2.700000000000000178, 1.600000000000000089 ) ) ;
#4226 = CARTESIAN_POINT ( 'NONE',  ( -2.043308330018790198, -0.5002118644067800046, 5.867646457774669422 ) ) ;
#4227 = CARTESIAN_POINT ( 'NONE',  ( -0.04278372834682089842, -3.729611093351540063, 2.346934926511239805 ) ) ;
#4228 = DIRECTION ( 'NONE',  ( -1.110223024625159992E-16, 0.000000000000000000, 1.000000000000000000 ) ) ;
#4229 = PLANE ( 'NONE',  #11529 ) ;
#4230 = CARTESIAN_POINT ( 'NONE',  ( -2.614198783383141045, -5.533262711864405325, 4.243032045539295360 ) ) ;
#4231 = ORIENTED_EDGE ( 'NONE', *, *, #11624, .F. ) ;
#4232 = EDGE_LOOP ( 'NONE', ( #15122, #5278, #8292, #15026, #9377, #4506, #743, #9277, #4667, #10100, #2665, #17005, #5084, #11412, #1796, #2920, #6120, #18045 ) ) ;
#4233 = PLANE ( 'NONE',  #2992 ) ;
#4234 = CARTESIAN_POINT ( 'NONE',  ( -1.899999999999999911, 0.5999999999999999778, 1.600000000000000089 ) ) ;
#4235 = CARTESIAN_POINT ( 'NONE',  ( 1.399999999999999911, 0.5999999999999999778, 6.100000000000000533 ) ) ;
#4236 = ORIENTED_EDGE ( 'NONE', *, *, #10102, .T. ) ;
#4237 = CARTESIAN_POINT ( 'NONE',  ( -1.351547610267091581, -1.517223705964159786, 6.983951126925262542 ) ) ;
#4238 = CARTESIAN_POINT ( 'NONE',  ( 1.112057765673850174, -5.020626044399135068, 2.286633591154370482 ) ) ;
#4239 = PLANE ( 'NONE',  #13363 ) ;
#4240 = CARTESIAN_POINT ( 'NONE',  ( -1.219286470748949913, -1.218316834576380181, 6.712979431025680732 ) ) ;
#4241 = DIRECTION ( 'NONE',  ( 0.000000000000000000, 0.000000000000000000, 1.000000000000000000 ) ) ;
#4242 = CARTESIAN_POINT ( 'NONE',  ( 2.343457872958619959, -4.148800282540729967, 4.916681529328559286 ) ) ;
#4243 = CARTESIAN_POINT ( 'NONE',  ( 4.898587196589409994E-17, 0.1000000000000000056, 8.300000000000000711 ) ) ;
#4244 = CARTESIAN_POINT ( 'NONE',  ( -2.029711248330079876, -3.380286769027221805, 4.391497016172549728 ) ) ;
#4245 = DIRECTION ( 'NONE',  ( 1.000000000000000000, 0.000000000000000000, 2.220446049250309876E-16 ) ) ;
#4246 = VERTEX_POINT ( 'NONE', #112 ) ;
#4247 = CARTESIAN_POINT ( 'NONE',  ( -0.7101077586918816964, -0.2831443699174400752, 2.770804889310179764 ) ) ;
#4248 = ORIENTED_EDGE ( 'NONE', *, *, #8347, .T. ) ;
#4249 = APPLICATION_CONTEXT ( 'automotive_design' ) ;
#4250 = EDGE_CURVE ( 'NONE', #3782, #14849, #5758, .T. ) ;
#4251 = CARTESIAN_POINT ( 'NONE',  ( -1.836970198721025435E-17, 6.700000000000000178, 6.850000000000000533 ) ) ;
#4252 = VERTEX_POINT ( 'NONE', #6870 ) ;
#4253 = EDGE_CURVE ( 'NONE', #3214, #15169, #4798, .T. ) ;
#4254 = FACE_OUTER_BOUND ( 'NONE', #18088, .T. ) ;
#4255 = EDGE_LOOP ( 'NONE', ( #12305, #7340, #6947, #11853 ) ) ;
#4256 = AXIS2_PLACEMENT_3D ( 'NONE', #10529, #10355, #4985 ) ;
#4257 = CARTESIAN_POINT ( 'NONE',  ( 1.695509042132770761, -5.046398305084744962, 3.542446458728613301 ) ) ;
#4258 = DIRECTION ( 'NONE',  ( -1.000000000000000000, 2.220446049250309876E-16, -8.269460797427580527E-16 ) ) ;
#4259 = CARTESIAN_POINT ( 'NONE',  ( 1.769280637098189946, -0.6409077950170640747, 2.931315639931909800 ) ) ;
#4260 = CARTESIAN_POINT ( 'NONE',  ( 2.500000000000000000, 9.199999999999999289, 0.6099999999999999867 ) ) ;
#4261 = DIRECTION ( 'NONE',  ( -1.110223024625159992E-16, 0.000000000000000000, -1.000000000000000000 ) ) ;
#4262 = LINE ( 'NONE', #15582, #15919 ) ;
#4263 = LINE ( 'NONE', #15583, #7367 ) ;
#4264 = CARTESIAN_POINT ( 'NONE',  ( -1.816660071039029933, -3.170692174432619748, 6.196159040268240936 ) ) ;
#4265 = CARTESIAN_POINT ( 'NONE',  ( -2.052456847059610734, -3.034803321062870651, 4.748194746458554327 ) ) ;
#4266 = CARTESIAN_POINT ( 'NONE',  ( 2.022304719220918479, -0.06673728813559356987, 4.346496488058688712 ) ) ;
#4267 = EDGE_CURVE ( 'NONE', #15324, #2153, #9969, .T. ) ;
#4268 = CARTESIAN_POINT ( 'NONE',  ( 2.088297318559229954, -0.3978813559322040283, 5.785136623276629919 ) ) ;
#4269 = DIRECTION ( 'NONE',  ( -6.123233995736769734E-17, 3.749399456654650178E-33, -1.000000000000000000 ) ) ;
#4270 = CARTESIAN_POINT ( 'NONE',  ( -1.949083719010310078, -0.5402542372881364852, 4.055210292801460170 ) ) ;
#4271 = DIRECTION ( 'NONE',  ( -4.318427418585891014E-15, 2.220446049250309876E-16, -1.000000000000000000 ) ) ;
#4272 = VERTEX_POINT ( 'NONE', #4715 ) ;
#4273 = EDGE_CURVE ( 'NONE', #1993, #2692, #10107, .T. ) ;
#4274 = CARTESIAN_POINT ( 'NONE',  ( 0.1910247150515120007, -0.004449152542373194588, 2.655937705488500722 ) ) ;
#4275 = CARTESIAN_POINT ( 'NONE',  ( -2.308170020371289599, -1.726818300558750074, 5.159452766389659217 ) ) ;
#4276 = ORIENTED_EDGE ( 'NONE', *, *, #1000, .T. ) ;
#4277 = EDGE_CURVE ( 'NONE', #17446, #17990, #6105, .T. ) ;
#4278 = EDGE_CURVE ( 'NONE', #3539, #138, #9054, .T. ) ;
#4279 = EDGE_LOOP ( 'NONE', ( #9149, #15954, #3002, #15617 ) ) ;
#4280 = CARTESIAN_POINT ( 'NONE',  ( -1.214457691476030332, -1.730659176918720510, 2.684103622926371280 ) ) ;
#4281 = CARTESIAN_POINT ( 'NONE',  ( -5.421010862427522170E-17, -2.500000000000000000, -2.168404344971008868E-16 ) ) ;
#4282 = CARTESIAN_POINT ( 'NONE',  ( 2.171642826483958899, -5.404237288135596451, 6.225392547715717484 ) ) ;
#4283 = EDGE_LOOP ( 'NONE', ( #9913, #5730, #13015, #18242, #5041, #8159, #7055, #1705, #18261, #8124, #13963, #1536, #17691, #6887, #14369, #10316, #8144, #2107, #9987 ) ) ;
#4284 = CARTESIAN_POINT ( 'NONE',  ( 2.350542563031990273, -1.004881363621820123, 4.817027120179740329 ) ) ;
#4285 = CARTESIAN_POINT ( 'NONE',  ( 0.5137283630188955730, -0.4379237288135597317, 6.687652957477222770 ) ) ;
#4286 = ORIENTED_EDGE ( 'NONE', *, *, #5296, .F. ) ;
#4287 = CARTESIAN_POINT ( 'NONE',  ( -1.149999999999999911, 9.299999999999998934, 7.500000000000000000 ) ) ;
#4288 = CARTESIAN_POINT ( 'NONE',  ( 1.899999999999999911, 0.5999999999999999778, 6.599999999999999645 ) ) ;
#4289 = DIRECTION ( 'NONE',  ( -1.000000000000000000, 1.480297366166869931E-15, 0.000000000000000000 ) ) ;
#4290 = CARTESIAN_POINT ( 'NONE',  ( 1.658519201881180738, -2.402178660919109365, 3.489952108543023623 ) ) ;
#4291 = DIRECTION ( 'NONE',  ( 0.000000000000000000, 0.000000000000000000, 1.000000000000000000 ) ) ;
#4292 = CARTESIAN_POINT ( 'NONE',  ( 2.645377369053839356, -0.3711864406779670222, 4.488260618344900088 ) ) ;
#4293 = ORIENTED_EDGE ( 'NONE', *, *, #11615, .F. ) ;
#4294 = PLANE ( 'NONE',  #17200 ) ;
#4295 = CARTESIAN_POINT ( 'NONE',  ( 1.000000000000000000, -7.000000000000000000, 3.700000000000000178 ) ) ;
#4296 = EDGE_CURVE ( 'NONE', #14130, #10006, #17290, .T. ) ;
#4297 = ORIENTED_EDGE ( 'NONE', *, *, #320, .T. ) ;
#4298 = CARTESIAN_POINT ( 'NONE',  ( -0.7046366965007886396, -4.911779243796845051, 2.768871435390180213 ) ) ;
#4299 = CARTESIAN_POINT ( 'NONE',  ( 2.286166334984490067, -5.386440677966100488, 5.258525443163859947 ) ) ;
#4300 = ORIENTED_EDGE ( 'NONE', *, *, #11315, .T. ) ;
#4301 = CARTESIAN_POINT ( 'NONE',  ( 1.248294325655349590, -0.02669491525423759587, 2.704938983774301420 ) ) ;
#4302 = CARTESIAN_POINT ( 'NONE',  ( 0.9150601050661639757, -5.430932203389830626, 6.868218666554230190 ) ) ;
#4303 = LINE ( 'NONE', #11530, #2884 ) ;
#4304 = ORIENTED_EDGE ( 'NONE', *, *, #11770, .F. ) ;
#4305 = DIRECTION ( 'NONE',  ( -1.734723475976809806E-16, 1.000000000000000000, 0.000000000000000000 ) ) ;
#4306 = CARTESIAN_POINT ( 'NONE',  ( 2.036228139452630259, -2.126560077819629857, 3.519948877554369915 ) ) ;
#4307 = EDGE_CURVE ( 'NONE', #13650, #6378, #2031, .T. ) ;
#4308 = FACE_OUTER_BOUND ( 'NONE', #718, .T. ) ;
#4309 = CARTESIAN_POINT ( 'NONE',  ( -2.052456847059610734, -3.034803321062870651, 4.748194746458554327 ) ) ;
#4310 = AXIS2_PLACEMENT_3D ( 'NONE', #8425, #15562, #176 ) ;
#4311 = DIRECTION ( 'NONE',  ( -1.000000000000000000, -9.028005242978079560E-48, 6.123233995736769734E-17 ) ) ;
#4312 = ORIENTED_EDGE ( 'NONE', *, *, #13870, .F. ) ;
#4313 = EDGE_CURVE ( 'NONE', #8096, #7005, #7631, .T. ) ;
#4314 = DIRECTION ( 'NONE',  ( 1.000000000000000000, 0.000000000000000000, 0.000000000000000000 ) ) ;
#4315 = CARTESIAN_POINT ( 'NONE',  ( -1.031876288691620625, -0.4690677966101705065, 7.145012538880312292 ) ) ;
#4316 = CARTESIAN_POINT ( 'NONE',  ( -0.09706517602693919000, -2.961097579838030125, 7.051451474958980725 ) ) ;
#4317 = CARTESIAN_POINT ( 'NONE',  ( -1.149999999999999911, 6.472933199251450276, 6.846017351831609865 ) ) ;
#4318 = DIRECTION ( 'NONE',  ( -1.000000000000000000, 0.000000000000000000, 0.000000000000000000 ) ) ;
#4319 = CARTESIAN_POINT ( 'NONE',  ( 0.5609751937345880402, -5.139830508474575232, 7.293870047334757523 ) ) ;
#4320 = VERTEX_POINT ( 'NONE', #6204 ) ;
#4321 = ORIENTED_EDGE ( 'NONE', *, *, #205, .T. ) ;
#4322 = LINE ( 'NONE', #9804, #10968 ) ;
#4323 = DIRECTION ( 'NONE',  ( -1.306144734853129823E-16, 1.000000000000000000, 0.000000000000000000 ) ) ;
#4324 = ORIENTED_EDGE ( 'NONE', *, *, #2700, .F. ) ;
#4325 = AXIS2_PLACEMENT_3D ( 'NONE', #3428, #6761, #9080 ) ;
#4326 = CARTESIAN_POINT ( 'NONE',  ( -2.281778813005780115, -4.847448931189379806, 5.276394947932169899 ) ) ;
#4327 = FACE_OUTER_BOUND ( 'NONE', #5387, .T. ) ;
#4328 = DIRECTION ( 'NONE',  ( 0.3420201433256691015, 0.000000000000000000, 0.9396926207859082059 ) ) ;
#4329 = PLANE ( 'NONE',  #1257 ) ;
#4330 = CARTESIAN_POINT ( 'NONE',  ( 1.460675875430079929, -0.9155690868286359141, 6.545310725710029587 ) ) ;
#4331 = VECTOR ( 'NONE', #7224, 1000.000000000000000 ) ;
#4332 = LINE ( 'NONE', #13890, #800 ) ;
#4333 = CARTESIAN_POINT ( 'NONE',  ( -0.8986180677147959095, -3.636457940198390304, 2.524860635301629852 ) ) ;
#4334 = CARTESIAN_POINT ( 'NONE',  ( -0.5999999999999999778, 10.80000000000000071, 7.599999999999999645 ) ) ;
#4335 = CYLINDRICAL_SURFACE ( 'NONE', #9993, 0.2500000000000002220 ) ;
#4336 = CARTESIAN_POINT ( 'NONE',  ( 0.7128755192781456307, -3.822764246504686270, 2.774718115017441367 ) ) ;
#4337 = AXIS2_PLACEMENT_3D ( 'NONE', #13400, #12204, #18009 ) ;
#4338 = FACE_OUTER_BOUND ( 'NONE', #2189, .T. ) ;
#4339 = VECTOR ( 'NONE', #3224, 1000.000000000000000 ) ;
#4340 = VECTOR ( 'NONE', #14871, 1000.000000000000000 ) ;
#4341 = VERTEX_POINT ( 'NONE', #195 ) ;
#4342 = CARTESIAN_POINT ( 'NONE',  ( -1.399999999999999911, -6.000000000000000000, 3.299999999999999822 ) ) ;
#4343 = ORIENTED_EDGE ( 'NONE', *, *, #8822, .F. ) ;
#4344 = CARTESIAN_POINT ( 'NONE',  ( -1.875000000000000000, 2.296212748401290437E-16, 7.700000000000000178 ) ) ;
#4345 = VERTEX_POINT ( 'NONE', #11860 ) ;
#4346 = DIRECTION ( 'NONE',  ( 1.224646799147350002E-16, -1.000000000000000000, -6.123233995736769734E-17 ) ) ;
#4347 = AXIS2_PLACEMENT_3D ( 'NONE', #7837, #10710, #6726 ) ;
#4348 = EDGE_CURVE ( 'NONE', #1875, #10826, #15758, .T. ) ;
#4349 = EDGE_CURVE ( 'NONE', #4874, #15355, #12377, .T. ) ;
#4350 = ORIENTED_EDGE ( 'NONE', *, *, #17509, .F. ) ;
#4351 = CARTESIAN_POINT ( 'NONE',  ( -1.980638384804660257, -5.237711864406785267, 4.159858630563765480 ) ) ;
#4352 = VECTOR ( 'NONE', #10594, 1000.000000000000000 ) ;
#4353 = LINE ( 'NONE', #10017, #6735 ) ;
#4354 = VECTOR ( 'NONE', #11735, 1000.000000000000000 ) ;
#4355 = DIRECTION ( 'NONE',  ( 0.000000000000000000, 0.000000000000000000, -1.000000000000000000 ) ) ;
#4356 = CARTESIAN_POINT ( 'NONE',  ( -1.899999999999999911, 4.700000000000000178, 0.6099999999999999867 ) ) ;
#4357 = DIRECTION ( 'NONE',  ( 1.000000000000000000, 0.000000000000000000, -7.401486830834370362E-16 ) ) ;
#4358 = DIRECTION ( 'NONE',  ( -1.000000000000000000, 0.000000000000000000, 0.000000000000000000 ) ) ;
#4359 = DIRECTION ( 'NONE',  ( -1.000000000000000000, 0.000000000000000000, 0.000000000000000000 ) ) ;
#4360 = ADVANCED_FACE ( 'NONE', ( #8709 ), #14354, .F. ) ;
#4361 = CARTESIAN_POINT ( 'NONE',  ( -2.283153923255329953, -3.403575057315510133, 4.129076318403500423 ) ) ;
#4362 = VECTOR ( 'NONE', #5889, 1000.000000000000000 ) ;
#4363 = CARTESIAN_POINT ( 'NONE',  ( -1.658519201881210714, -3.197821339080880065, 3.489952108543053377 ) ) ;
#4364 = VECTOR ( 'NONE', #2161, 1000.000000000000000 ) ;
#4365 = DIRECTION ( 'NONE',  ( 0.000000000000000000, 0.000000000000000000, -1.000000000000000000 ) ) ;
#4366 = DIRECTION ( 'NONE',  ( 0.000000000000000000, 0.000000000000000000, 1.000000000000000000 ) ) ;
#4367 = ORIENTED_EDGE ( 'NONE', *, *, #7004, .T. ) ;
#4368 = AXIS2_PLACEMENT_3D ( 'NONE', #17992, #14766, #3556 ) ;
#4369 = CARTESIAN_POINT ( 'NONE',  ( 0.7476103186298468373, -0.01779661016949178609, 2.787995836256459636 ) ) ;
#4370 = CARTESIAN_POINT ( 'NONE',  ( 1.526791597786429922, -2.774791273531720392, 6.490992212270249695 ) ) ;
#4371 = VERTEX_POINT ( 'NONE', #17478 ) ;
#4372 = FACE_OUTER_BOUND ( 'NONE', #3661, .T. ) ;
#4373 = EDGE_LOOP ( 'NONE', ( #825, #7346, #9497, #5202 ) ) ;
#4374 = CARTESIAN_POINT ( 'NONE',  ( 2.091095264232529338, -3.943046564306110113, 5.779845490516200890 ) ) ;
#4375 = SHAPE_DEFINITION_REPRESENTATION ( #8328, #2757 ) ;
#4376 = CARTESIAN_POINT ( 'NONE',  ( -0.07299321914061848715, -5.598516949152539723, 2.350000000000000089 ) ) ;
#4377 = STYLED_ITEM ( 'NONE', ( #15382 ), #8014 ) ;
#4378 = VECTOR ( 'NONE', #1385, 1000.000000000000000 ) ;
#4379 = VERTEX_POINT ( 'NONE', #8803 ) ;
#4380 = EDGE_CURVE ( 'NONE', #6428, #13183, #14622, .T. ) ;
#4381 = CARTESIAN_POINT ( 'NONE',  ( 0.3265524029357661506, -0.4423728813559331119, 6.726831181542982208 ) ) ;
#4382 = PRODUCT_DEFINITION ( 'UNKNOWN', '', #4119, #5473 ) ;
#4383 = ORIENTED_EDGE ( 'NONE', *, *, #11612, .F. ) ;
#4384 = EDGE_CURVE ( 'NONE', #475, #7297, #11573, .T. ) ;
#4385 = VECTOR ( 'NONE', #9784, 1000.000000000000000 ) ;
#4386 = DIRECTION ( 'NONE',  ( 0.000000000000000000, 0.000000000000000000, 1.000000000000000000 ) ) ;
#4387 = CARTESIAN_POINT ( 'NONE',  ( 0.9000000000000000222, -10.00000000000000000, 3.799999999999999822 ) ) ;
#4388 = EDGE_CURVE ( 'NONE', #17710, #103, #12973, .T. ) ;
#4389 = CARTESIAN_POINT ( 'NONE',  ( 1.599895119336370852, -2.728214696955149510, 5.986560317183676538 ) ) ;
#4390 = ADVANCED_FACE ( 'NONE', ( #4616, #560, #5934, #10180 ), #1774, .F. ) ;
#4391 = CARTESIAN_POINT ( 'NONE',  ( 0.2469343877495150108, -0.3044491525423730915, 2.057675570509529539 ) ) ;
#4392 = ORIENTED_EDGE ( 'NONE', *, *, #11047, .F. ) ;
#4393 = DIRECTION ( 'NONE',  ( 2.537652627714639929E-16, 1.000000000000000000, 0.000000000000000000 ) ) ;
#4394 = VECTOR ( 'NONE', #10498, 1000.000000000000000 ) ;
#4395 = DIRECTION ( 'NONE',  ( 1.000000000000000000, 9.028005242978079560E-48, -6.123233995736769734E-17 ) ) ;
#4396 =( GEOMETRIC_REPRESENTATION_CONTEXT ( 3 ) GLOBAL_UNCERTAINTY_ASSIGNED_CONTEXT ( ( #5299 ) ) GLOBAL_UNIT_ASSIGNED_CONTEXT ( ( #13099, #4837, #14651 ) ) REPRESENTATION_CONTEXT ( 'NONE', 'WORKASPACE' ) );
#4397 = ORIENTED_EDGE ( 'NONE', *, *, #16070, .T. ) ;
#4398 = CARTESIAN_POINT ( 'NONE',  ( 0.03000000000000110217, 11.40000000000000036, 7.649999999999999467 ) ) ;
#4399 = CARTESIAN_POINT ( 'NONE',  ( 2.155845792290829621, -5.355296610169490101, 3.756158857535770057 ) ) ;
#4400 = AXIS2_PLACEMENT_3D ( 'NONE', #6798, #5406, #4003 ) ;
#4401 = CARTESIAN_POINT ( 'NONE',  ( 0.1749999999999999889, 8.200000000000001066, -3.200000000000000178 ) ) ;
#4402 = DIRECTION ( 'NONE',  ( -1.000000000000000000, 0.000000000000000000, 0.000000000000000000 ) ) ;
#4403 = VERTEX_POINT ( 'NONE', #10276 ) ;
#4404 = CARTESIAN_POINT ( 'NONE',  ( -0.1749999999999999889, 7.900000000000000355, 0.4000000000000000222 ) ) ;
#4405 = AXIS2_PLACEMENT_3D ( 'NONE', #13663, #4942, #14763 ) ;
#4406 = CARTESIAN_POINT ( 'NONE',  ( 0.2564439965879030114, -1.055298816558370101, 7.039440566481209416 ) ) ;
#4407 = EDGE_CURVE ( 'NONE', #2448, #7602, #4896, .T. ) ;
#4408 = CARTESIAN_POINT ( 'NONE',  ( -1.899999999999999911, 9.199999999999999289, 1.600000000000000089 ) ) ;
#4409 = CARTESIAN_POINT ( 'NONE',  ( -0.5302109551885640926, -1.800524041783588824, 2.716624547488271979 ) ) ;
#4410 = DIRECTION ( 'NONE',  ( 0.000000000000000000, 0.000000000000000000, 1.000000000000000000 ) ) ;
#4411 = CARTESIAN_POINT ( 'NONE',  ( -3.161120280659493168E-15, -5.600000000000000533, 2.050000000000001155 ) ) ;
#4412 = EDGE_LOOP ( 'NONE', ( #8223, #8414, #8474, #9171 ) ) ;
#4413 = LINE ( 'NONE', #1737, #12972 ) ;
#4414 = CARTESIAN_POINT ( 'NONE',  ( -2.519547246525518425, -0.5402542372881364852, 3.866491354109200529 ) ) ;
#4415 = VECTOR ( 'NONE', #844, 1000.000000000000000 ) ;
#4416 = CARTESIAN_POINT ( 'NONE',  ( -2.296954468777729463, -4.963890372630819670, 4.187412587068699565 ) ) ;
#4417 = FACE_OUTER_BOUND ( 'NONE', #4540, .T. ) ;
#4418 = FACE_OUTER_BOUND ( 'NONE', #6515, .T. ) ;
#4419 = CARTESIAN_POINT ( 'NONE',  ( 2.224278379903029901, -5.090889830508480429, 5.468825643806100700 ) ) ;
#4420 = VERTEX_POINT ( 'NONE', #1856 ) ;
#4421 = VERTEX_POINT ( 'NONE', #7503 ) ;
#4422 = CARTESIAN_POINT ( 'NONE',  ( 0.8740908734716299477, 4.154758922476410099, 7.700000000000000178 ) ) ;
#4423 = PLANE ( 'NONE',  #17962 ) ;
#4424 = ORIENTED_EDGE ( 'NONE', *, *, #10848, .T. ) ;
#4425 = CARTESIAN_POINT ( 'NONE',  ( -2.325590009395030133, -4.870737219477670799, 5.061077271074069905 ) ) ;
#4426 = EDGE_CURVE ( 'NONE', #7267, #13803, #4999, .T. ) ;
#4427 = CARTESIAN_POINT ( 'NONE',  ( 1.330034674284700458, -0.7763906680874423927, 3.132218110693851809 ) ) ;
#4428 = CARTESIAN_POINT ( 'NONE',  ( -2.500000000000000000, 9.199999999999999289, 1.600000000000000089 ) ) ;
#4429 = VECTOR ( 'NONE', #722, 1000.000000000000000 ) ;
#4430 = CARTESIAN_POINT ( 'NONE',  ( -2.100188519621619676, -1.590929447189000090, 3.637948273607420013 ) ) ;
#4431 = DIRECTION ( 'NONE',  ( -0.6614378277661479011, 3.218725199566341288E-16, -0.7499999999999997780 ) ) ;
#4432 = CARTESIAN_POINT ( 'NONE',  ( 2.262450597846779932, -4.195376859117310175, 5.348122657979680561 ) ) ;
#4433 = DIRECTION ( 'NONE',  ( -1.000000000000000000, 0.000000000000000000, 0.000000000000000000 ) ) ;
#4434 = ADVANCED_BREP_SHAPE_REPRESENTATION ( '', ( #8014, #17681 ), #12094 ) ;
#4435 = CARTESIAN_POINT ( 'NONE',  ( 1.741179788930650840, -4.265241723982168942, 5.787747574231955738 ) ) ;
#4436 = DIRECTION ( 'NONE',  ( 1.000000000000000000, 0.000000000000000000, -5.332141831895923026E-16 ) ) ;
#4437 = CARTESIAN_POINT ( 'NONE',  ( -1.449568901432419343, -0.5625000000000005551, 3.250431098567584165 ) ) ;
#4438 = VERTEX_POINT ( 'NONE', #5089 ) ;
#4439 = CARTESIAN_POINT ( 'NONE',  ( -1.899999999999999911, 4.700000000000000178, 1.600000000000000089 ) ) ;
#4440 = EDGE_LOOP ( 'NONE', ( #11659, #5141, #5944, #3237 ) ) ;
#4441 = CIRCLE ( 'NONE', #5631, 0.2999999999999999334 ) ;
#4442 = DIRECTION ( 'NONE',  ( 0.000000000000000000, 6.123233995736769734E-17, -1.000000000000000000 ) ) ;
#4443 = VERTEX_POINT ( 'NONE', #10832 ) ;
#4444 = CARTESIAN_POINT ( 'NONE',  ( -1.921786527979019166, -5.542161016949150643, 3.977907449687794195 ) ) ;
#4445 = CARTESIAN_POINT ( 'NONE',  ( -0.2683982510037440927, -3.407415933675483899, 2.059720455735791322 ) ) ;
#4446 =( NAMED_UNIT ( * ) SI_UNIT ( $, .STERADIAN. ) SOLID_ANGLE_UNIT ( ) );
#4447 = CARTESIAN_POINT ( 'NONE',  ( 1.670747152266691016, -0.4963810343603142217, 3.047345280935851441 ) ) ;
#4448 = CARTESIAN_POINT ( 'NONE',  ( 2.500000000000000000, 11.15000000000000036, 1.600000000000000089 ) ) ;
#4449 = CARTESIAN_POINT ( 'NONE',  ( -1.652654650382400003, -4.804713230972780025, 3.029252778805629820 ) ) ;
#4450 = LINE ( 'NONE', #2800, #1409 ) ;
#4451 = DIRECTION ( 'NONE',  ( 1.899065700016719806E-16, 1.000000000000000000, 0.000000000000000000 ) ) ;
#4452 = AXIS2_PLACEMENT_3D ( 'NONE', #1451, #6823, #18085 ) ;
#4453 = CARTESIAN_POINT ( 'NONE',  ( 0.3413183941262679655, -2.914521003261450360, 7.028571974690709823 ) ) ;
#4454 = CARTESIAN_POINT ( 'NONE',  ( -0.6713553523422816083, -2.732055573315119723, 6.640150466718877098 ) ) ;
#4455 = CARTESIAN_POINT ( 'NONE',  ( 1.846259792136599076, -0.05338983050847485173, 3.802221692020924415 ) ) ;
#4456 = LINE ( 'NONE', #1685, #8511 ) ;
#4457 = CARTESIAN_POINT ( 'NONE',  ( 1.899999999999999911, 11.40000000000000036, 1.600000000000000089 ) ) ;
#4458 = EDGE_LOOP ( 'NONE', ( #4072, #1609, #13207, #988 ) ) ;
#4459 = CARTESIAN_POINT ( 'NONE',  ( -1.818868030982659700, -3.244397915657463827, 2.767428454397828919 ) ) ;
#4460 = CARTESIAN_POINT ( 'NONE',  ( -2.332582362116870200, -0.2313559322033900134, 4.387643303570819775 ) ) ;
#4461 = CARTESIAN_POINT ( 'NONE',  ( 1.687170344132030042, -2.751502985243429844, 6.340793075730549511 ) ) ;
#4462 = ORIENTED_EDGE ( 'NONE', *, *, #12422, .F. ) ;
#4463 = ORIENTED_EDGE ( 'NONE', *, *, #4380, .T. ) ;
#4464 = CARTESIAN_POINT ( 'NONE',  ( -1.764807890102219501, -3.221109627369170170, 3.143016121304770039 ) ) ;
#4465 = CARTESIAN_POINT ( 'NONE',  ( 2.625437065641401446, -5.081991525423726230, 5.087214675345139270 ) ) ;
#4466 = EDGE_LOOP ( 'NONE', ( #15778, #10124, #4686, #12944 ) ) ;
#4467 = CARTESIAN_POINT ( 'NONE',  ( 1.921786527979010062, -0.3578389830508479363, 3.977907449687776431 ) ) ;
#4468 = ORIENTED_EDGE ( 'NONE', *, *, #15265, .T. ) ;
#4469 = PLANE ( 'NONE',  #198 ) ;
#4470 = DIRECTION ( 'NONE',  ( 6.938893903907229610E-17, 0.000000000000000000, 1.000000000000000000 ) ) ;
#4471 = CARTESIAN_POINT ( 'NONE',  ( -1.750352751699820963, -1.913124606865061139, 3.627075451280493468 ) ) ;
#4472 = EDGE_LOOP ( 'NONE', ( #6604, #12984, #6336, #4690 ) ) ;
#4473 = LINE ( 'NONE', #1711, #15468 ) ;
#4474 = CARTESIAN_POINT ( 'NONE',  ( -0.1749999999999999889, 6.799999999999999822, 1.600000000000000089 ) ) ;
#4475 = CARTESIAN_POINT ( 'NONE',  ( -0.2453710345350140487, -0.4557203389830515317, 6.738252723719333481 ) ) ;
#4476 = ORIENTED_EDGE ( 'NONE', *, *, #11676, .F. ) ;
#4477 = DIRECTION ( 'NONE',  ( 1.000000000000000000, 0.000000000000000000, 0.000000000000000000 ) ) ;
#4478 = CARTESIAN_POINT ( 'NONE',  ( -1.754713504580578842, -5.551059322033894183, 3.634325740584633646 ) ) ;
#4479 = LINE ( 'NONE', #10135, #15925 ) ;
#4480 = ADVANCED_FACE ( 'NONE', ( #5282 ), #16298, .F. ) ;
#4481 = CARTESIAN_POINT ( 'NONE',  ( -1.943632316591239473, -0.2536016949152540279, 3.373048379518170936 ) ) ;
#4482 = EDGE_CURVE ( 'NONE', #17750, #3610, #10740, .T. ) ;
#4483 = FACE_OUTER_BOUND ( 'NONE', #1214, .T. ) ;
#4484 = ORIENTED_EDGE ( 'NONE', *, *, #8374, .F. ) ;
#4485 = DIRECTION ( 'NONE',  ( 0.000000000000000000, 0.000000000000000000, 1.000000000000000000 ) ) ;
#4486 = CARTESIAN_POINT ( 'NONE',  ( -1.397172971746989845, -1.707370888630439953, 2.806153814454939610 ) ) ;
#4487 = CARTESIAN_POINT ( 'NONE',  ( 0.6628679656440349399, 6.450000000000000178, 1.670710678118660031 ) ) ;
#4488 = CARTESIAN_POINT ( 'NONE',  ( 0.8259795455966094657, -2.545749267008810435, 6.579537079411867495 ) ) ;
#4489 = VECTOR ( 'NONE', #8246, 1000.000000000000000 ) ;
#4490 = LINE ( 'NONE', #7466, #11748 ) ;
#4491 = ORIENTED_EDGE ( 'NONE', *, *, #5731, .F. ) ;
#4492 = EDGE_CURVE ( 'NONE', #7436, #15079, #10828, .T. ) ;
#4493 = CARTESIAN_POINT ( 'NONE',  ( -1.149999999999999911, 9.274118095489749081, 7.596592582628910684 ) ) ;
#4494 = CARTESIAN_POINT ( 'NONE',  ( 0.4221287159901364605, -0.4423728813559331119, 7.320050063945812369 ) ) ;
#4495 = CARTESIAN_POINT ( 'NONE',  ( 2.342931736853870017, -4.102223705964150646, 4.477701633099130163 ) ) ;
#4496 = CARTESIAN_POINT ( 'NONE',  ( -0.1749999999999999889, 9.099999999999999645, 0.5999999999999999778 ) ) ;
#4497 = CARTESIAN_POINT ( 'NONE',  ( 2.350000000000000089, -5.599999999999999645, 2.799999999999999822 ) ) ;
#4498 = CARTESIAN_POINT ( 'NONE',  ( -1.925836318347889931, -5.188771186440680694, 6.525927015348141680 ) ) ;
#4499 = ORIENTED_EDGE ( 'NONE', *, *, #7928, .F. ) ;
#4500 = EDGE_CURVE ( 'NONE', #14793, #15397, #17660, .T. ) ;
#4501 = VERTEX_POINT ( 'NONE', #933 ) ;
#4502 = DIRECTION ( 'NONE',  ( -8.326672684688679970E-16, 0.000000000000000000, -1.000000000000000000 ) ) ;
#4503 = EDGE_CURVE ( 'NONE', #8531, #13096, #17843, .T. ) ;
#4504 =( LENGTH_UNIT ( ) NAMED_UNIT ( * ) SI_UNIT ( .MILLI., .METRE. ) );
#4505 = CARTESIAN_POINT ( 'NONE',  ( -1.889999999999999902, 4.100000000000000533, -6.851683986394989688E-16 ) ) ;
#4506 = ORIENTED_EDGE ( 'NONE', *, *, #5071, .T. ) ;
#4507 = CARTESIAN_POINT ( 'NONE',  ( -2.543624461644929724, -1.703530012270459970, 5.457025951420040322 ) ) ;
#4508 = PLANE ( 'NONE',  #2605 ) ;
#4509 = LINE ( 'NONE', #4588, #4354 ) ;
#4510 = B_SPLINE_CURVE_WITH_KNOTS ( 'NONE', 3,
 ( #13406, #9037, #1715, #8741, #7877, #15018, #14826, #13631, #12234, #941, #7694, #6579, #14919, #12047, #14389, #7369 ),
 .UNSPECIFIED., .F., .F.,
 ( 4, 1, 1, 1, 1, 1, 1, 1, 1, 1, 1, 1, 1, 4 ),
 ( 0.4999998211434326656, 0.5106244842457859923, 0.5531978902116679864, 0.5957712970450619316, 0.6383447191100900531, 0.6809180289764420468, 0.7234918990885960133, 0.7660634153086809395, 0.8086437809559909873, 0.8511815656861039248, 0.8935997744639799789, 0.9363910903529559793, 0.9718312009674719976, 1.000000000000000000 ),
 .UNSPECIFIED. ) ;
#4511 = CARTESIAN_POINT ( 'NONE',  ( 0.04278372834676710118, -1.870388906648450034, 2.346934926511239805 ) ) ;
#4512 = CARTESIAN_POINT ( 'NONE',  ( 1.449568901432419343, -5.337500000000000355, 3.250431098567584165 ) ) ;
#4513 = SHAPE_REPRESENTATION ( 'Actuator Return Helical Spring', ( #17681 ), #7087 ) ;
#4514 = CARTESIAN_POINT ( 'NONE',  ( -2.260671505268489145, -1.913124606865061139, 3.309864021662289435 ) ) ;
#4515 = DIRECTION ( 'NONE',  ( -1.000000000000000000, -4.037174635000570090E-16, 0.000000000000000000 ) ) ;
#4516 = CARTESIAN_POINT ( 'NONE',  ( -0.2220816246931631155, -4.544701183441625325, 6.740975647723836950 ) ) ;
#4517 = CARTESIAN_POINT ( 'NONE',  ( 0.9000000000000000222, 6.450000000000000178, 3.600000000000000089 ) ) ;
#4518 = LINE ( 'NONE', #369, #2968 ) ;
#4519 = ORIENTED_EDGE ( 'NONE', *, *, #2474, .T. ) ;
#4520 = ADVANCED_FACE ( 'NONE', ( #12036 ), #736, .F. ) ;
#4521 =( LENGTH_UNIT ( ) NAMED_UNIT ( * ) SI_UNIT ( .MILLI., .METRE. ) );
#4522 = EDGE_LOOP ( 'NONE', ( #18097, #7771, #2406, #3522 ) ) ;
#4523 = DIRECTION ( 'NONE',  ( 0.000000000000000000, 0.000000000000000000, 1.000000000000000000 ) ) ;
#4524 = VERTEX_POINT ( 'NONE', #6370 ) ;
#4525 = CARTESIAN_POINT ( 'NONE',  ( -0.8731223871104993872, -5.470974576271190770, 6.558046933601121786 ) ) ;
#4526 = CARTESIAN_POINT ( 'NONE',  ( 1.883442729065728960, -2.452596113855660676, 6.569694408006650832 ) ) ;
#4527 = DIRECTION ( 'NONE',  ( 1.233581138472399909E-16, 6.167905692361979821E-17, -1.000000000000000000 ) ) ;
#4528 = ADVANCED_FACE ( 'NONE', ( #3886 ), #9154, .F. ) ;
#4529 = CARTESIAN_POINT ( 'NONE',  ( 2.053221424930760097, -0.8651516338920849369, 3.549770689668250157 ) ) ;
#4530 = LINE ( 'NONE', #12976, #10314 ) ;
#4531 = CARTESIAN_POINT ( 'NONE',  ( -0.3159454637156809409, -2.984385868126319785, 7.032150113402090064 ) ) ;
#4532 = CARTESIAN_POINT ( 'NONE',  ( 0.6965028529799376367, -4.129352870612409632, 6.631265289497767057 ) ) ;
#4533 = CARTESIAN_POINT ( 'NONE',  ( -0.005674314996644000582, -5.239933087847700399, 2.472195840738729888 ) ) ;
#4534 = LINE ( 'NONE', #16210, #3523 ) ;
#4535 = VERTEX_POINT ( 'NONE', #9540 ) ;
#4536 = CARTESIAN_POINT ( 'NONE',  ( 2.260671505268459391, -3.686875393134939394, 3.309864021662241029 ) ) ;
#4537 = EDGE_CURVE ( 'NONE', #11911, #1590, #7867, .T. ) ;
#4538 = CARTESIAN_POINT ( 'NONE',  ( 0.1365430262726380628, -0.1468220338983061424, 6.748423079423377047 ) ) ;
#4539 = CARTESIAN_POINT ( 'NONE',  ( 1.902324933209389890, -2.402178660919109809, 3.314393441133530072 ) ) ;
#4540 = EDGE_LOOP ( 'NONE', ( #730, #18179, #4217, #8676 ) ) ;
#4541 = VERTEX_POINT ( 'NONE', #3691 ) ;
#4542 = CARTESIAN_POINT ( 'NONE',  ( -0.2365712905368978769, -3.407415933675479902, 2.358466376073659720 ) ) ;
#4543 = CARTESIAN_POINT ( 'NONE',  ( 0.000000000000000000, 0.000000000000000000, 0.000000000000000000 ) ) ;
#4544 = CARTESIAN_POINT ( 'NONE',  ( 2.630358833876468960, -5.068644067796615360, 4.347767980622404771 ) ) ;
#4545 = VERTEX_POINT ( 'NONE', #12138 ) ;
#4546 = LINE ( 'NONE', #3087, #5551 ) ;
#4547 = LINE ( 'NONE', #10386, #15004 ) ;
#4548 = ORIENTED_EDGE ( 'NONE', *, *, #659, .F. ) ;
#4549 = DIRECTION ( 'NONE',  ( 1.000000000000000000, 0.000000000000000000, 0.000000000000000000 ) ) ;
#4550 = CARTESIAN_POINT ( 'NONE',  ( -2.002297259025881182, -3.287133615874059611, 5.153549919110945510 ) ) ;
#4551 = CARTESIAN_POINT ( 'NONE',  ( 2.653602652190420574, -0.3756355932203404024, 4.735326402787084277 ) ) ;
#4552 = EDGE_LOOP ( 'NONE', ( #15513, #5009, #992, #17069, #3967, #15017 ) ) ;
#4553 = CARTESIAN_POINT ( 'NONE',  ( -0.8298945877350979439, -5.211074464177370302, 2.494426474263899962 ) ) ;
#4554 = CARTESIAN_POINT ( 'NONE',  ( 0.1749999999999999889, 9.299999999999998934, 0.4000000000000000222 ) ) ;
#4555 = DIRECTION ( 'NONE',  ( 2.220446049250309876E-16, 0.000000000000000000, -1.000000000000000000 ) ) ;
#4556 = ORIENTED_EDGE ( 'NONE', *, *, #14675, .F. ) ;
#4557 = LINE ( 'NONE', #17331, #2066 ) ;
#4558 = CARTESIAN_POINT ( 'NONE',  ( -1.821706171509118954, -5.502118644067805597, 5.646608543709410455 ) ) ;
#4559 = FILL_AREA_STYLE ('',( #15792 ) ) ;
#4560 = CARTESIAN_POINT ( 'NONE',  ( 0.009452110982654783611, -0.3001920447045380858, 2.050000000000001155 ) ) ;
#4561 = EDGE_CURVE ( 'NONE', #9915, #14122, #6685, .T. ) ;
#4562 = CARTESIAN_POINT ( 'NONE',  ( -0.7785957873162068221, -3.659746228486683073, 2.162894899107379754 ) ) ;
#4563 = ORIENTED_EDGE ( 'NONE', *, *, #1374, .T. ) ;
#4564 = ADVANCED_FACE ( 'NONE', ( #17758 ), #644, .F. ) ;
#4565 = CARTESIAN_POINT ( 'NONE',  ( -2.102728310581289950, -1.358046564306109927, 5.757014351541099195 ) ) ;
#4566 = DIRECTION ( 'NONE',  ( 0.000000000000000000, -1.000000000000000000, -1.586032892321649771E-16 ) ) ;
#4567 = CARTESIAN_POINT ( 'NONE',  ( 0.6470883152343921418, -2.569037555297099651, 6.648378442427241630 ) ) ;
#4568 = CARTESIAN_POINT ( 'NONE',  ( 0.1749999999999999889, 7.799999999999999822, 0.4000000000000000222 ) ) ;
#4569 = ORIENTED_EDGE ( 'NONE', *, *, #11877, .F. ) ;
#4570 = EDGE_CURVE ( 'NONE', #9728, #8493, #646, .T. ) ;
#4571 = CARTESIAN_POINT ( 'NONE',  ( -1.899999999999999911, 11.40000000000000036, 7.550000000000000711 ) ) ;
#4572 = CARTESIAN_POINT ( 'NONE',  ( 1.447263454062181598, -0.9388573751169233539, 6.924531903016430512 ) ) ;
#4573 = CARTESIAN_POINT ( 'NONE',  ( -1.670747221194380128, -5.103620102360550526, 3.047345349617600174 ) ) ;
#4574 = CARTESIAN_POINT ( 'NONE',  ( -1.875000000000000000, 2.296212748401290437E-16, 8.300000000000000711 ) ) ;
#4575 = PLANE ( 'NONE',  #11259 ) ;
#4576 = CARTESIAN_POINT ( 'NONE',  ( -2.645377369053839356, -5.228813559322024851, 4.488260618344918740 ) ) ;
#4577 = VERTEX_POINT ( 'NONE', #15008 ) ;
#4578 = ORIENTED_EDGE ( 'NONE', *, *, #7807, .T. ) ;
#4579 = LINE ( 'NONE', #17263, #16885 ) ;
#4580 = CARTESIAN_POINT ( 'NONE',  ( 1.899999999999999911, 4.700000000000000178, 1.600000000000000089 ) ) ;
#4581 = ORIENTED_EDGE ( 'NONE', *, *, #13884, .T. ) ;
#4582 = LINE ( 'NONE', #17457, #12689 ) ;
#4583 = CARTESIAN_POINT ( 'NONE',  ( -2.049607015837349167, -3.170692174432623744, 6.385889905549041679 ) ) ;
#4584 = APPLICATION_CONTEXT ( 'automotive_design' ) ;
#4585 = VECTOR ( 'NONE', #13058, 1000.000000000000000 ) ;
#4586 = ADVANCED_FACE ( 'NONE', ( #1023 ), #6659, .F. ) ;
#4587 = DIRECTION ( 'NONE',  ( 1.000000000000000000, 0.000000000000000000, 0.000000000000000000 ) ) ;
#4588 = CARTESIAN_POINT ( 'NONE',  ( 1.750000000000000000, 11.40000000000000036, 7.700000000000000178 ) ) ;
#4589 = CARTESIAN_POINT ( 'NONE',  ( 1.145304265383909836, -2.522460978720529656, 6.755972720436079548 ) ) ;
#4590 = EDGE_CURVE ( 'NONE', #16860, #1432, #12776, .T. ) ;
#4591 = PLANE ( 'NONE',  #17328 ) ;
#4592 = CARTESIAN_POINT ( 'NONE',  ( -2.325590009395030133, -4.870737219477670799, 5.061077271074069905 ) ) ;
#4593 = ADVANCED_FACE ( 'NONE', ( #8152 ), #4239, .T. ) ;
#4594 = FACE_OUTER_BOUND ( 'NONE', #10753, .T. ) ;
#4595 = EDGE_CURVE ( 'NONE', #11049, #8102, #5378, .T. ) ;
#4596 = CARTESIAN_POINT ( 'NONE',  ( 2.151546283159470274, -0.8884399221803740421, 3.746273477677459773 ) ) ;
#4597 = VECTOR ( 'NONE', #2713, 1000.000000000000000 ) ;
#4598 = DIRECTION ( 'NONE',  ( 0.000000000000000000, 0.000000000000000000, 1.000000000000000000 ) ) ;
#4599 = EDGE_CURVE ( 'NONE', #2341, #10479, #2685, .T. ) ;
#4600 = CARTESIAN_POINT ( 'NONE',  ( 1.000896394980339998, -0.4290254237288140260, 6.829956240957369751 ) ) ;
#4601 = DIRECTION ( 'NONE',  ( -1.000000000000000000, 0.000000000000000000, 0.000000000000000000 ) ) ;
#4602 = ORIENTED_EDGE ( 'NONE', *, *, #12870, .F. ) ;
#4603 = CIRCLE ( 'NONE', #14983, 0.5999999999999998668 ) ;
#4604 = AXIS2_PLACEMENT_3D ( 'NONE', #11144, #8106, #16798 ) ;
#4605 = CARTESIAN_POINT ( 'NONE',  ( 1.899999999999999911, 2.000000000000000000, -1.259531014076939845E-15 ) ) ;
#4606 = ORIENTED_EDGE ( 'NONE', *, *, #17581, .F. ) ;
#4607 = CARTESIAN_POINT ( 'NONE',  ( -1.399999999999999911, 0.5999999999999999778, 3.299999999999999822 ) ) ;
#4608 = FACE_OUTER_BOUND ( 'NONE', #4283, .T. ) ;
#4609 = ORIENTED_EDGE ( 'NONE', *, *, #4537, .T. ) ;
#4610 = CARTESIAN_POINT ( 'NONE',  ( 1.449568901432419343, -5.337500000000000355, 3.250431098567584165 ) ) ;
#4611 = CARTESIAN_POINT ( 'NONE',  ( 2.226511124464869873, -1.074746228486680000, 5.462491901673799610 ) ) ;
#4612 = CARTESIAN_POINT ( 'NONE',  ( -2.212163452524020357, -2.895073591333140239, 6.166099093621881799 ) ) ;
#4613 = EDGE_CURVE ( 'NONE', #15772, #6568, #16665, .T. ) ;
#4614 = SHAPE_REPRESENTATION ( 'Movable Sliding Contacts', ( #17681 ), #552 ) ;
#4615 = PLANE ( 'NONE',  #6400 ) ;
#4616 = FACE_BOUND ( 'NONE', #9216, .T. ) ;
#4617 = EDGE_CURVE ( 'NONE', #2627, #8501, #15470, .T. ) ;
#4618 = VECTOR ( 'NONE', #914, 1000.000000000000000 ) ;
#4619 = CARTESIAN_POINT ( 'NONE',  ( -1.250000000000000000, 0.5999999999999999778, 6.100000000000000533 ) ) ;
#4620 = LINE ( 'NONE', #10279, #7963 ) ;
#4621 = CARTESIAN_POINT ( 'NONE',  ( -2.281778813005780115, -4.847448931189379806, 5.276394947932169899 ) ) ;
#4622 = CARTESIAN_POINT ( 'NONE',  ( 1.491388273269019571, -4.012911429170968880, 6.110908523251506352 ) ) ;
#4623 = DIRECTION ( 'NONE',  ( 1.000000000000000000, 9.656020733808335804E-16, 0.000000000000000000 ) ) ;
#4624 = VECTOR ( 'NONE', #7851, 1000.000000000000000 ) ;
#4625 = VECTOR ( 'NONE', #3568, 1000.000000000000000 ) ;
#4626 = DIRECTION ( 'NONE',  ( -1.000000000000000000, 2.220446049250309876E-16, 6.123233995736769734E-17 ) ) ;
#4627 = VERTEX_POINT ( 'NONE', #11200 ) ;
#4628 = CARTESIAN_POINT ( 'NONE',  ( -1.468674196027810686, -4.362235753495300905, 6.910454658870877509 ) ) ;
#4629 = CARTESIAN_POINT ( 'NONE',  ( 0.6964468257805941365, -0.1334745762711869732, 6.631228347243847132 ) ) ;
#4630 = CARTESIAN_POINT ( 'NONE',  ( 2.245209214543399945, -2.635061543801989981, 5.405536158119010004 ) ) ;
#4631 = ORIENTED_EDGE ( 'NONE', *, *, #2467, .T. ) ;
#4632 = ORIENTED_EDGE ( 'NONE', *, *, #4865, .T. ) ;
#4633 = CARTESIAN_POINT ( 'NONE',  ( 0.02999999999999939868, 12.00000000000000000, 7.649999999999999467 ) ) ;
#4634 = VECTOR ( 'NONE', #7283, 1000.000000000000000 ) ;
#4635 = ORIENTED_EDGE ( 'NONE', *, *, #13771, .F. ) ;
#4636 = VECTOR ( 'NONE', #8270, 1000.000000000000000 ) ;
#4637 = CARTESIAN_POINT ( 'NONE',  ( 1.197297565406180153, -4.082776294035841858, 6.726135293448178842 ) ) ;
#4638 = DIRECTION ( 'NONE',  ( 0.000000000000000000, 0.000000000000000000, 1.000000000000000000 ) ) ;
#4639 = CARTESIAN_POINT ( 'NONE',  ( -1.925836318347889931, -5.188771186440680694, 6.525927015348141680 ) ) ;
#4640 = ORIENTED_EDGE ( 'NONE', *, *, #11175, .F. ) ;
#4641 = CARTESIAN_POINT ( 'NONE',  ( 2.500000000000000000, 0.8000000000000000444, -2.399999999999999911 ) ) ;
#4642 = AXIS2_PLACEMENT_3D ( 'NONE', #17963, #9559, #13914 ) ;
#4643 = CARTESIAN_POINT ( 'NONE',  ( 1.378221871957440170, -0.4201271186440679872, 6.607619368096269596 ) ) ;
#4644 = CIRCLE ( 'NONE', #7036, 0.01000000000000002623 ) ;
#4645 = ORIENTED_EDGE ( 'NONE', *, *, #2841, .T. ) ;
#4646 = VECTOR ( 'NONE', #9136, 1000.000000000000000 ) ;
#4647 = EDGE_CURVE ( 'NONE', #13169, #3824, #15283, .T. ) ;
#4648 = DIRECTION ( 'NONE',  ( -1.000000000000000000, 0.000000000000000000, 0.000000000000000000 ) ) ;
#4649 = CARTESIAN_POINT ( 'NONE',  ( 1.661700935788380074, -5.337500000000000355, 3.038299064211610112 ) ) ;
#4650 = LINE ( 'NONE', #1878, #1719 ) ;
#4651 = CARTESIAN_POINT ( 'NONE',  ( -2.051695471449629160, -3.333710192450643373, 4.773807418740784847 ) ) ;
#4652 = CARTESIAN_POINT ( 'NONE',  ( 2.638803263991410741, -0.08008474576271243373, 4.982085668537405532 ) ) ;
#4653 = AXIS2_PLACEMENT_3D ( 'NONE', #16152, #2177, #13373 ) ;
#4654 = ORIENTED_EDGE ( 'NONE', *, *, #12073, .T. ) ;
#4655 = CARTESIAN_POINT ( 'NONE',  ( -1.229686204202100175, -5.164643153926309793, 2.674737924334550154 ) ) ;
#4656 = VECTOR ( 'NONE', #10515, 1000.000000000000000 ) ;
#4657 = LINE ( 'NONE', #10313, #9099 ) ;
#4658 = ADVANCED_BREP_SHAPE_REPRESENTATION ( '', ( #7985, #17681 ), #12699 ) ;
#4659 = VERTEX_POINT ( 'NONE', #6760 ) ;
#4660 = CARTESIAN_POINT ( 'NONE',  ( 1.399999999999999911, -7.000000000000000000, 3.299999999999999822 ) ) ;
#4661 = CARTESIAN_POINT ( 'NONE',  ( -1.489797906646480596, -5.488771186440680516, 6.112509577910826941 ) ) ;
#4662 = CARTESIAN_POINT ( 'NONE',  ( 0.1749999999999999889, 7.700000000000000178, 1.600000000000000089 ) ) ;
#4663 = VECTOR ( 'NONE', #18291, 1000.000000000000000 ) ;
#4664 = PLANE ( 'NONE',  #2691 ) ;
#4665 = VECTOR ( 'NONE', #14540, 1000.000000000000000 ) ;
#4666 = CARTESIAN_POINT ( 'NONE',  ( 2.470260739716200860, -4.032358841099289215, 3.729986819255199926 ) ) ;
#4667 = ORIENTED_EDGE ( 'NONE', *, *, #15207, .T. ) ;
#4668 = CIRCLE ( 'NONE', #13548, 0.7000000000000000666 ) ;
#4669 = AXIS2_PLACEMENT_3D ( 'NONE', #16543, #13753, #6249 ) ;
#4670 = CARTESIAN_POINT ( 'NONE',  ( 2.159566522375460096, -2.359442960702510028, 5.635424033751039730 ) ) ;
#4671 = CARTESIAN_POINT ( 'NONE',  ( 2.500000000000000000, 0.7500000000000000000, 7.649999999999999467 ) ) ;
#4672 = LINE ( 'NONE', #8934, #450 ) ;
#4673 = AXIS2_PLACEMENT_3D ( 'NONE', #10724, #3490, #818 ) ;
#4674 = CARTESIAN_POINT ( 'NONE',  ( 2.002297259025890064, -2.312866384125929820, 5.153549919110900213 ) ) ;
#4675 = VECTOR ( 'NONE', #9381, 1000.000000000000000 ) ;
#4676 = FACE_OUTER_BOUND ( 'NONE', #7393, .T. ) ;
#4677 = ORIENTED_EDGE ( 'NONE', *, *, #17430, .T. ) ;
#4678 = DIRECTION ( 'NONE',  ( 0.000000000000000000, 6.123233995736769734E-17, -1.000000000000000000 ) ) ;
#4679 = CARTESIAN_POINT ( 'NONE',  ( -1.576846334488060553, -1.707370888630439065, 2.565364356520430267 ) ) ;
#4680 = ORIENTED_EDGE ( 'NONE', *, *, #13128, .T. ) ;
#4681 = CARTESIAN_POINT ( 'NONE',  ( 2.343457872958619959, -4.148800282540729967, 4.916681529328559286 ) ) ;
#4682 = DIRECTION ( 'NONE',  ( 1.224646799147350002E-16, -0.9659258262890690894, -0.2588190451025180749 ) ) ;
#4683 = LINE ( 'NONE', #17177, #9778 ) ;
#4684 = CARTESIAN_POINT ( 'NONE',  ( 1.467041701146838406, -5.122033898305085486, 6.911479965439912831 ) ) ;
#4685 = ORIENTED_EDGE ( 'NONE', *, *, #5316, .T. ) ;
#4686 = ORIENTED_EDGE ( 'NONE', *, *, #16963, .F. ) ;
#4687 = LINE ( 'NONE', #17181, #5937 ) ;
#4688 = VECTOR ( 'NONE', #1734, 1000.000000000000000 ) ;
#4689 = CARTESIAN_POINT ( 'NONE',  ( -0.7500000000000000000, 6.450000000000000178, 3.200000000000000178 ) ) ;
#4690 = ORIENTED_EDGE ( 'NONE', *, *, #1266, .T. ) ;
#4691 = CARTESIAN_POINT ( 'NONE',  ( 1.315254646989809872, -2.821367850108300157, 7.005042061779697349 ) ) ;
#4692 =( GEOMETRIC_REPRESENTATION_CONTEXT ( 3 ) GLOBAL_UNCERTAINTY_ASSIGNED_CONTEXT ( ( #9735 ) ) GLOBAL_UNIT_ASSIGNED_CONTEXT ( ( #1648, #11831, #15812 ) ) REPRESENTATION_CONTEXT ( 'NONE', 'WORKASPACE' ) );
#4693 = CARTESIAN_POINT ( 'NONE',  ( -3.760880495917719358E-15, -5.299999999999999822, 2.350000000000000089 ) ) ;
#4694 = DIRECTION ( 'NONE',  ( 2.220446049250309876E-16, 1.000000000000000000, 8.874685183736369893E-32 ) ) ;
#4695 = CARTESIAN_POINT ( 'NONE',  ( -1.687170344131989852, -2.848497014756560475, 6.340793075730589479 ) ) ;
#4696 = CARTESIAN_POINT ( 'NONE',  ( 0.9866023595736967966, -5.020626044399130627, 2.560054107758459985 ) ) ;
#4697 = CARTESIAN_POINT ( 'NONE',  ( -2.612083973477999699, -1.819971453711898945, 4.230818789270855085 ) ) ;
#4698 = VECTOR ( 'NONE', #7077, 1000.000000000000000 ) ;
#4699 = FACE_OUTER_BOUND ( 'NONE', #15626, .T. ) ;
#4700 = CARTESIAN_POINT ( 'NONE',  ( -1.272929729338609262, -4.684430913171365063, 6.310761232086878003 ) ) ;
#4701 = CARTESIAN_POINT ( 'NONE',  ( 0.3743405594629510280, -0.4423728813559330009, 7.023440622744399953 ) ) ;
#4702 = LINE ( 'NONE', #10437, #6197 ) ;
#4703 = EDGE_LOOP ( 'NONE', ( #13029, #11339, #10061, #7714 ) ) ;
#4704 = PLANE ( 'NONE',  #4256 ) ;
#4705 = ORIENTED_EDGE ( 'NONE', *, *, #556, .T. ) ;
#4706 = CARTESIAN_POINT ( 'NONE',  ( -0.7500000000000000000, 3.050000000000000266, 3.200000000000000178 ) ) ;
#4707 = CARTESIAN_POINT ( 'NONE',  ( 1.399999999999999911, 0.5999999999999999778, 6.100000000000000533 ) ) ;
#4708 = EDGE_CURVE ( 'NONE', #3214, #6864, #12410, .T. ) ;
#4709 = ORIENTED_EDGE ( 'NONE', *, *, #155, .F. ) ;
#4710 = EDGE_CURVE ( 'NONE', #229, #17764, #16844, .T. ) ;
#4711 = VECTOR ( 'NONE', #15476, 1000.000000000000000 ) ;
#4712 = ADVANCED_FACE ( 'NONE', ( #1377 ), #5735, .F. ) ;
#4713 = CARTESIAN_POINT ( 'NONE',  ( 2.337178851518220135, -2.588484967225419986, 4.976298214796759822 ) ) ;
#4714 = FACE_OUTER_BOUND ( 'NONE', #4950, .T. ) ;
#4715 = CARTESIAN_POINT ( 'NONE',  ( -1.000000000000000000, 5.400000000000000355, 8.300000000000000711 ) ) ;
#4716 = CARTESIAN_POINT ( 'NONE',  ( -1.981271652668300298, -1.633665147405599871, 5.970160748022450115 ) ) ;
#4717 = CARTESIAN_POINT ( 'NONE',  ( -0.04278372834682089842, -3.729611093351540063, 2.346934926511239805 ) ) ;
#4718 = CARTESIAN_POINT ( 'NONE',  ( 1.485933537025759366, -0.8030495317899833951, 3.286232459959989249 ) ) ;
#4719 = LINE ( 'NONE', #16303, #15627 ) ;
#4720 = CIRCLE ( 'NONE', #13618, 0.09999999999999990841 ) ;
#4721 = DIRECTION ( 'NONE',  ( 1.306144734853129823E-16, -1.000000000000000000, -1.306144734853129823E-16 ) ) ;
#4722 = ORIENTED_EDGE ( 'NONE', *, *, #5750, .T. ) ;
#4723 = ADVANCED_FACE ( 'NONE', ( #15386 ), #4329, .T. ) ;
#4724 = CARTESIAN_POINT ( 'NONE',  ( -1.432215783582709401, -0.1868644067796619845, 6.170863372171116801 ) ) ;
#4725 = CARTESIAN_POINT ( 'NONE',  ( 1.869848057046569867, -4.288530012270459935, 6.129130480762009725 ) ) ;
#4726 = ORIENTED_EDGE ( 'NONE', *, *, #8918, .F. ) ;
#4727 = VERTEX_POINT ( 'NONE', #9812 ) ;
#4728 = DIRECTION ( 'NONE',  ( -0.2800000000000001377, 0.9599999999999999645, 0.000000000000000000 ) ) ;
#4729 = EDGE_CURVE ( 'NONE', #9457, #16402, #16747, .T. ) ;
#4730 = VERTEX_POINT ( 'NONE', #4060 ) ;
#4731 = CARTESIAN_POINT ( 'NONE',  ( -1.303621121494419777, -4.362235753495302681, 6.659417683669698995 ) ) ;
#4732 = EDGE_CURVE ( 'NONE', #5832, #10396, #1484, .T. ) ;
#4733 = CONTEXT_DEPENDENT_SHAPE_REPRESENTATION ( #12533, #14956 ) ;
#4734 = CARTESIAN_POINT ( 'NONE',  ( -1.554165089654128584, -5.179872881355935377, 6.851145244874527584 ) ) ;
#4735 = PLANE ( 'NONE',  #228 ) ;
#4736 = VECTOR ( 'NONE', #9307, 1000.000000000000000 ) ;
#4737 = CARTESIAN_POINT ( 'NONE',  ( 0.4000000000000000222, -1.399999999999999911, 5.100000000000000533 ) ) ;
#4738 = ORIENTED_EDGE ( 'NONE', *, *, #4426, .T. ) ;
#4739 = EDGE_CURVE ( 'NONE', #13665, #5243, #2778, .T. ) ;
#4740 = CARTESIAN_POINT ( 'NONE',  ( 1.736825397686149852, -3.985782264522713447, 3.605313112995111702 ) ) ;
#4741 = CARTESIAN_POINT ( 'NONE',  ( 1.875000000000000000, 11.25000000000000000, 8.300000000000000711 ) ) ;
#4742 = CARTESIAN_POINT ( 'NONE',  ( 2.484260633728970546, -0.05783898305084796132, 3.766563288620793593 ) ) ;
#4743 = VERTEX_POINT ( 'NONE', #7 ) ;
#4744 = CARTESIAN_POINT ( 'NONE',  ( 0.2189795514005130062, -0.3044491525423729805, 2.356806637999009801 ) ) ;
#4745 = VERTEX_POINT ( 'NONE', #5648 ) ;
#4746 = AXIS2_PLACEMENT_3D ( 'NONE', #751, #3706, #13256 ) ;
#4747 = CARTESIAN_POINT ( 'NONE',  ( 0.009452039534070141164, -0.3001931771041043140, 2.350000000173209092 ) ) ;
#4748 = DIRECTION ( 'NONE',  ( 0.000000000000000000, 0.000000000000000000, 1.000000000000000000 ) ) ;
#4749 = EDGE_CURVE ( 'NONE', #17050, #8650, #2521, .T. ) ;
#4750 = DIRECTION ( 'NONE',  ( 1.000000000000000000, 4.157615153618229646E-15, 0.000000000000000000 ) ) ;
#4751 = CARTESIAN_POINT ( 'NONE',  ( -2.523518139275819916, -3.263845327585779277, 5.521565513971835593 ) ) ;
#4752 = VERTEX_POINT ( 'NONE', #9901 ) ;
#4753 = CARTESIAN_POINT ( 'NONE',  ( -0.2365712905368979879, -3.407415933675480346, 2.358466376073659720 ) ) ;
#4754 = EDGE_CURVE ( 'NONE', #10130, #15477, #2865, .T. ) ;
#4755 = DIRECTION ( 'NONE',  ( -6.049014748177262516E-16, -8.531426931033445878E-16, -1.000000000000000000 ) ) ;
#4756 = LINE ( 'NONE', #17341, #11972 ) ;
#4757 = CARTESIAN_POINT ( 'NONE',  ( -1.683529720875190705, -4.455388906648449776, 5.875001924065656134 ) ) ;
#4758 = PLANE ( 'NONE',  #17638 ) ;
#4759 = CARTESIAN_POINT ( 'NONE',  ( -1.503314099254069447, -1.660794312053860633, 3.301805249040033363 ) ) ;
#4760 = ORIENTED_EDGE ( 'NONE', *, *, #14335, .F. ) ;
#4761 = DIRECTION ( 'NONE',  ( 0.000000000000000000, 0.000000000000000000, -1.000000000000000000 ) ) ;
#4762 = CARTESIAN_POINT ( 'NONE',  ( 1.000000000000000000, -6.000000000000000000, 3.299999999999999822 ) ) ;
#4763 = CARTESIAN_POINT ( 'NONE',  ( -2.607432201095288615, -1.521064582324129777, 4.205620581240213873 ) ) ;
#4764 = ORIENTED_EDGE ( 'NONE', *, *, #2474, .F. ) ;
#4765 = CARTESIAN_POINT ( 'NONE',  ( 2.313035575219750228, -4.172088570829020071, 5.134294963419709923 ) ) ;
#4766 = DIRECTION ( 'NONE',  ( -1.224646799147350002E-16, 1.000000000000000000, 6.123233995736769734E-17 ) ) ;
#4767 = DIRECTION ( 'NONE',  ( 0.000000000000000000, 2.220446049250309876E-16, -1.000000000000000000 ) ) ;
#4768 = CARTESIAN_POINT ( 'NONE',  ( -1.549742865090599997, -5.184322033898309812, 6.471102547561460305 ) ) ;
#4769 = EDGE_LOOP ( 'NONE', ( #16400, #10079, #5642, #13980 ) ) ;
#4770 = EDGE_CURVE ( 'NONE', #10029, #2905, #91, .T. ) ;
#4771 = ORIENTED_EDGE ( 'NONE', *, *, #13003, .F. ) ;
#4772 = LINE ( 'NONE', #3381, #5354 ) ;
#4773 =( NAMED_UNIT ( * ) PLANE_ANGLE_UNIT ( ) SI_UNIT ( $, .RADIAN. ) );
#4774 = CARTESIAN_POINT ( 'NONE',  ( -0.6628679656440360501, 3.050000000000000266, 1.670710678118650261 ) ) ;
#4775 = ORIENTED_EDGE ( 'NONE', *, *, #14135, .T. ) ;
#4776 = CARTESIAN_POINT ( 'NONE',  ( -2.479511223993290603, -1.866548030288480042, 3.753882785753710483 ) ) ;
#4777 = EDGE_CURVE ( 'NONE', #1639, #240, #6059, .T. ) ;
#4778 = CARTESIAN_POINT ( 'NONE',  ( 0.5637478356992829953, -0.6606104644819250638, 2.398845082743519708 ) ) ;
#4779 = DIRECTION ( 'NONE',  ( -0.000000000000000000, 1.000000000000000000, 0.000000000000000000 ) ) ;
#4780 = CARTESIAN_POINT ( 'NONE',  ( -1.115198193348240219, -4.338947465207009913, 6.772457159276569882 ) ) ;
#4781 = VECTOR ( 'NONE', #9207, 1000.000000000000000 ) ;
#4782 = CARTESIAN_POINT ( 'NONE',  ( 1.151392222988870895, -5.028306595106930565, 2.990827770388080342 ) ) ;
#4783 = CARTESIAN_POINT ( 'NONE',  ( 1.853635285637830865, -1.191187669928120529, 6.599249831075482575 ) ) ;
#4784 = CARTESIAN_POINT ( 'NONE',  ( -1.399999999999999911, 6.400000000000000355, 8.300000000000000711 ) ) ;
#4785 = CARTESIAN_POINT ( 'NONE',  ( 1.699999999999999956, 2.299999999999999822, 7.599999999999999645 ) ) ;
#4786 = DIRECTION ( 'NONE',  ( -1.000000000000000000, 2.381191005321109844E-32, 0.000000000000000000 ) ) ;
#4787 = DIRECTION ( 'NONE',  ( 1.224646799147340881E-16, 1.000000000000000000, 0.000000000000000000 ) ) ;
#4788 = ORIENTED_EDGE ( 'NONE', *, *, #12474, .F. ) ;
#4789 = LINE ( 'NONE', #10640, #6032 ) ;
#4790 = EDGE_LOOP ( 'NONE', ( #5247, #4764, #4886, #9134, #9211, #455, #615, #5862 ) ) ;
#4791 = CYLINDRICAL_SURFACE ( 'NONE', #17330, 0.2750000000000000222 ) ;
#4792 = CARTESIAN_POINT ( 'NONE',  ( -1.899999999999999911, 11.40000000000000036, 0.5999999999999999778 ) ) ;
#4793 = ORIENTED_EDGE ( 'NONE', *, *, #6329, .F. ) ;
#4794 = EDGE_CURVE ( 'NONE', #18164, #37, #4756, .T. ) ;
#4795 = CARTESIAN_POINT ( 'NONE',  ( -2.345213174852959881, -1.796683165423619943, 4.503223853122380049 ) ) ;
#4796 = DIRECTION ( 'NONE',  ( -6.123233995736767268E-17, 0.000000000000000000, -1.000000000000000000 ) ) ;
#4797 = CARTESIAN_POINT ( 'NONE',  ( 1.718313768400149932, -0.5108663019338149924, 2.998025103714370143 ) ) ;
#4798 = LINE ( 'NONE', #4448, #3733 ) ;
#4799 = CARTESIAN_POINT ( 'NONE',  ( 2.231116159141619981, -0.9117282104686620370, 3.951089877392439664 ) ) ;
#4800 = CARTESIAN_POINT ( 'NONE',  ( -1.781655196750479897, -3.520016498756949996, 3.162323035427820450 ) ) ;
#4801 = CARTESIAN_POINT ( 'NONE',  ( 1.436030008293490701, -1.191187669928120529, 6.167214932417436124 ) ) ;
#4802 = PRODUCT_RELATED_PRODUCT_CATEGORY ( 'part', '', ( #12599 ) ) ;
#4803 = CARTESIAN_POINT ( 'NONE',  ( 0.5889081234606849957, -0.4379237288135600092, 6.978529000034869867 ) ) ;
#4804 = DIRECTION ( 'NONE',  ( 1.000000000000000000, 0.000000000000000000, 1.556829778943089964E-16 ) ) ;
#4805 = EDGE_CURVE ( 'NONE', #1785, #17654, #7254, .T. ) ;
#4806 = CARTESIAN_POINT ( 'NONE',  ( 0.5500000000000000444, 7.799999999999999822, 3.600000000000000089 ) ) ;
#4807 = VERTEX_POINT ( 'NONE', #780 ) ;
#4808 = CARTESIAN_POINT ( 'NONE',  ( 1.088937603231269646, -0.3266949152542383272, 2.959627624143540192 ) ) ;
#4809 = CARTESIAN_POINT ( 'NONE',  ( -2.349464193210359930, -3.356998480738930368, 4.563019372514619754 ) ) ;
#4810 = VERTEX_POINT ( 'NONE', #6154 ) ;
#4811 = ORIENTED_EDGE ( 'NONE', *, *, #13193, .T. ) ;
#4812 = FACE_OUTER_BOUND ( 'NONE', #3282, .T. ) ;
#4813 = ORIENTED_EDGE ( 'NONE', *, *, #16166, .F. ) ;
#4814 = CYLINDRICAL_SURFACE ( 'NONE', #4746, 0.3999999999999999667 ) ;
#4815 = ITEM_DEFINED_TRANSFORMATION ( 'NONE', 'NONE', #9731,  #17681 ) ;
#4816 = CARTESIAN_POINT ( 'NONE',  ( -0.4221287159901280228, -5.157627118644064979, 7.320050063945812369 ) ) ;
#4817 = LINE ( 'NONE', #14558, #9385 ) ;
#4818 = CARTESIAN_POINT ( 'NONE',  ( -2.058670345754650022, -0.5491525423728820243, 3.559656372813929881 ) ) ;
#4819 = ORIENTED_EDGE ( 'NONE', *, *, #6530, .T. ) ;
#4820 = EDGE_CURVE ( 'NONE', #13610, #2948, #4672, .T. ) ;
#4821 = CARTESIAN_POINT ( 'NONE',  ( -1.399999999999999911, -6.000000000000000000, 3.299999999999999822 ) ) ;
#4822 = LINE ( 'NONE', #14742, #7334 ) ;
#4823 = CARTESIAN_POINT ( 'NONE',  ( 1.217499609005879613, -3.892629111369556139, 3.046943272389411206 ) ) ;
#4824 = EDGE_CURVE ( 'NONE', #1993, #1835, #10490, .T. ) ;
#4825 = EDGE_CURVE ( 'NONE', #5242, #17654, #2969, .T. ) ;
#4826 = CARTESIAN_POINT ( 'NONE',  ( 2.645377369053839356, -0.07118644067796667252, 4.488260618344900088 ) ) ;
#4827 = ORIENTED_EDGE ( 'NONE', *, *, #8684, .T. ) ;
#4828 = CARTESIAN_POINT ( 'NONE',  ( 0.8570167067220200163, -0.3177966101694920664, 2.508190348879349774 ) ) ;
#4829 = EDGE_CURVE ( 'NONE', #14423, #5781, #7727, .T. ) ;
#4830 = ADVANCED_FACE ( 'NONE', ( #5036 ), #14760, .T. ) ;
#4831 = EDGE_LOOP ( 'NONE', ( #12548, #9706, #13268, #6034 ) ) ;
#4832 = CARTESIAN_POINT ( 'NONE',  ( 1.747582379783020778, -0.4156779661016956062, 6.697200745122486865 ) ) ;
#4833 = EDGE_CURVE ( 'NONE', #5409, #7679, #12085, .T. ) ;
#4834 = ORIENTED_EDGE ( 'NONE', *, *, #1797, .T. ) ;
#4835 = LINE ( 'NONE', #9187, #6222 ) ;
#4836 = CARTESIAN_POINT ( 'NONE',  ( 0.2812789908084389889, -5.444279661016950378, 7.036533610117280624 ) ) ;
#4837 =( NAMED_UNIT ( * ) PLANE_ANGLE_UNIT ( ) SI_UNIT ( $, .RADIAN. ) );
#4838 = CARTESIAN_POINT ( 'NONE',  ( 1.899999999999999911, 10.00000000000000000, 1.600000000000000089 ) ) ;
#4839 = CARTESIAN_POINT ( 'NONE',  ( -1.494590226124050014, -0.2673043920988010247, 2.870965838437660178 ) ) ;
#4840 = CARTESIAN_POINT ( 'NONE',  ( -2.502804106625960756, -3.426863345603793576, 3.817341913956430410 ) ) ;
#4841 = ORIENTED_EDGE ( 'NONE', *, *, #9045, .F. ) ;
#4842 = CARTESIAN_POINT ( 'NONE',  ( 1.044181395669780077, -3.547145663405210314, 2.590869634085890105 ) ) ;
#4843 = EDGE_CURVE ( 'NONE', #15809, #4957, #11899, .T. ) ;
#4844 = DIRECTION ( 'NONE',  ( -0.6614378277661479011, 3.218725199566341288E-16, -0.7499999999999997780 ) ) ;
#4845 = DIRECTION ( 'NONE',  ( 0.000000000000000000, 0.000000000000000000, 1.000000000000000000 ) ) ;
#4846 = CARTESIAN_POINT ( 'NONE',  ( 1.919159680931818990, -3.733451969711523155, 3.970803207828129455 ) ) ;
#4848 = EDGE_CURVE ( 'NONE', #15692, #3854, #7542, .T. ) ;
#4847 = CARTESIAN_POINT ( 'NONE',  ( -1.875000000000000000, 0.7500000000000000000, 7.700000000000000178 ) ) ;
#4849 = CARTESIAN_POINT ( 'NONE',  ( 1.399999999999999911, -9.500000000000000000, 6.100000000000000533 ) ) ;
#4850 = CARTESIAN_POINT ( 'NONE',  ( 1.549925137359331462, -0.8689925102520592581, 6.046340934239826659 ) ) ;
#4851 = EDGE_LOOP ( 'NONE', ( #14290, #1439, #7605, #6489 ) ) ;
#4852 = CARTESIAN_POINT ( 'NONE',  ( 1.000000000000000000, -7.000000000000000000, 5.700000000000000178 ) ) ;
#4853 = CARTESIAN_POINT ( 'NONE',  ( 1.835211330903820937, -0.8922807985403484743, 6.617058440403981834 ) ) ;
#4854 = VERTEX_POINT ( 'NONE', #17438 ) ;
#4855 = LINE ( 'NONE', #17805, #7064 ) ;
#4856 = LINE ( 'NONE', #4496, #15202 ) ;
#4857 = CARTESIAN_POINT ( 'NONE',  ( -1.250000000000000000, 0.5999999999999999778, 7.599999999999999645 ) ) ;
#4858 = CARTESIAN_POINT ( 'NONE',  ( -1.851073041990159984, -5.193220338983049800, 6.153284478378270528 ) ) ;
#4859 = ORIENTED_EDGE ( 'NONE', *, *, #16310, .T. ) ;
#4860 = ORIENTED_EDGE ( 'NONE', *, *, #11178, .F. ) ;
#4861 = PLANE ( 'NONE',  #4162 ) ;
#4862 = CARTESIAN_POINT ( 'NONE',  ( -1.149999999999999911, 6.447051294741199534, 6.942609934460510779 ) ) ;
#4863 = CARTESIAN_POINT ( 'NONE',  ( 1.000000000000000000, -7.000000000000000000, 3.700000000000000178 ) ) ;
#4864 = ORIENTED_EDGE ( 'NONE', *, *, #8470, .F. ) ;
#4865 = EDGE_CURVE ( 'NONE', #6673, #3787, #1571, .T. ) ;
#4866 = DIRECTION ( 'NONE',  ( -4.265713465516724418E-16, -1.000000000000000000, 0.000000000000000000 ) ) ;
#4867 = CARTESIAN_POINT ( 'NONE',  ( -1.963178672446121098, -1.959701183441630024, 2.914210764660470687 ) ) ;
#4868 = CARTESIAN_POINT ( 'NONE',  ( 1.800000000000000044, 7.799999999999999822, 1.600000000000000089 ) ) ;
#4869 = CARTESIAN_POINT ( 'NONE',  ( 1.600000000000000089, 3.147362922373949982E-16, 4.000000000000000000 ) ) ;
#4870 = CARTESIAN_POINT ( 'NONE',  ( 2.182690844914370043, -3.919758276017820453, 5.580117243900430068 ) ) ;
#4872 = EDGE_CURVE ( 'NONE', #8624, #8561, #17518, .T. ) ;
#4871 = CARTESIAN_POINT ( 'NONE',  ( 1.147638118088980086, -5.328211948015596278, 2.987995008461610702 ) ) ;
#4874 = VERTEX_POINT ( 'NONE', #6322 ) ;
#4873 = CARTESIAN_POINT ( 'NONE',  ( -2.349129089426440054, -4.894025507765950245, 4.842612091679129982 ) ) ;
#4875 = DIRECTION ( 'NONE',  ( 0.000000000000000000, -1.000000000000000000, 0.000000000000000000 ) ) ;
#4876 = DIRECTION ( 'NONE',  ( 1.554023113895890109E-14, -1.000000000000000000, -1.110223024626929998E-16 ) ) ;
#4877 = CARTESIAN_POINT ( 'NONE',  ( 2.253200202764420013, -0.3889830508474579895, 5.379408587037500133 ) ) ;
#4878 = PLANE ( 'NONE',  #5327 ) ;
#4879 = CARTESIAN_POINT ( 'NONE',  ( -2.203023580853999963, -5.542161016949149754, 3.872235369154300333 ) ) ;
#4880 = ORIENTED_EDGE ( 'NONE', *, *, #7126, .F. ) ;
#4881 = PRODUCT ( 'Actuator Spring Stop Clip', 'Actuator Spring Stop Clip', '', ( #1794 ) ) ;
#4882 = FACE_OUTER_BOUND ( 'NONE', #900, .T. ) ;
#4883 = ORIENTED_EDGE ( 'NONE', *, *, #9718, .T. ) ;
#4884 = DIRECTION ( 'NONE',  ( 0.000000000000000000, 0.000000000000000000, -1.000000000000000000 ) ) ;
#4885 = CARTESIAN_POINT ( 'NONE',  ( 0.5999999999999999778, 11.40000000000000036, 7.700000000000000178 ) ) ;
#4886 = ORIENTED_EDGE ( 'NONE', *, *, #14388, .T. ) ;
#4887 = CARTESIAN_POINT ( 'NONE',  ( 0.2365712905368450025, -2.192584066324519743, 2.358466376073659720 ) ) ;
#4888 = DIRECTION ( 'NONE',  ( -6.344131569286580347E-16, -1.000000000000000000, 1.586032892321649771E-16 ) ) ;
#4889 = CARTESIAN_POINT ( 'NONE',  ( 0.4974685680287860290, -5.439830508474580384, 7.000224381598740386 ) ) ;
#4890 = CARTESIAN_POINT ( 'NONE',  ( -1.899999999999999911, 2.664535259100380036E-16, 9.955530934770520091 ) ) ;
#4891 = CARTESIAN_POINT ( 'NONE',  ( 1.803891155489780074, -0.8185750573155089471, 3.188470185434109982 ) ) ;
#4892 = CARTESIAN_POINT ( 'NONE',  ( 1.994983296312400123, -4.265241723982169830, 5.948514050749290405 ) ) ;
#4893 = CARTESIAN_POINT ( 'NONE',  ( 1.996236309555640798, -1.051457940198389673, 5.179523137126535559 ) ) ;
#4894 = CIRCLE ( 'NONE', #16435, 0.2750000000000000222 ) ;
#4895 = LINE ( 'NONE', #16209, #246 ) ;
#4896 = CIRCLE ( 'NONE', #5513, 0.1999999999999996503 ) ;
#4897 = LINE ( 'NONE', #11582, #11520 ) ;
#4898 = EDGE_LOOP ( 'NONE', ( #15119, #2518, #15485, #12345 ) ) ;
#4899 = DIRECTION ( 'NONE',  ( 0.000000000000000000, -0.4472135954999631458, 0.8944271909999133019 ) ) ;
#4900 = CARTESIAN_POINT ( 'NONE',  ( -2.000624272291700034, -0.2358050847457631438, 4.239366054776020576 ) ) ;
#4901 = CARTESIAN_POINT ( 'NONE',  ( 2.102728310581320148, -4.241953435693879726, 5.757014351541050345 ) ) ;
#4902 = VERTEX_POINT ( 'NONE', #10406 ) ;
#4903 = ORIENTED_EDGE ( 'NONE', *, *, #13611, .T. ) ;
#4904 = DIRECTION ( 'NONE',  ( -1.000000000000000000, 0.000000000000000000, 0.000000000000000000 ) ) ;
#4905 = ORIENTED_EDGE ( 'NONE', *, *, #14101, .T. ) ;
#4906 = CARTESIAN_POINT ( 'NONE',  ( 0.5500000000000000444, 3.050000000000000266, 3.200000000000000178 ) ) ;
#4907 = CARTESIAN_POINT ( 'NONE',  ( -2.306642602145299925, -5.215466101694909540, 5.166805192608490138 ) ) ;
#4908 = VECTOR ( 'NONE', #7918, 1000.000000000000000 ) ;
#4909 = CARTESIAN_POINT ( 'NONE',  ( 0.7500000000000000000, 6.450000000000000178, 2.699264068711930253 ) ) ;
#4910 = CARTESIAN_POINT ( 'NONE',  ( 0.5889081234606849957, -0.4379237288135600092, 6.978529000034869867 ) ) ;
#4911 = ORIENTED_EDGE ( 'NONE', *, *, #199, .T. ) ;
#4912 = DIRECTION ( 'NONE',  ( -1.000000000000000000, 0.000000000000000000, -4.440892098500630106E-16 ) ) ;
#4913 = CARTESIAN_POINT ( 'NONE',  ( 2.053018524985070314, -4.125511994252439862, 4.695903819313355321 ) ) ;
#4914 = VECTOR ( 'NONE', #3940, 1000.000000000000000 ) ;
#4915 = CARTESIAN_POINT ( 'NONE',  ( 1.610878918935058524, -0.03114406779661053892, 2.590989782159081933 ) ) ;
#4916 = EDGE_LOOP ( 'NONE', ( #8813, #17383, #3006, #13142 ) ) ;
#4917 = VECTOR ( 'NONE', #14522, 1000.000000000000000 ) ;
#4918 = CARTESIAN_POINT ( 'NONE',  ( -2.171642826483958899, -0.4957627118644069575, 6.225392547715731695 ) ) ;
#4919 = VECTOR ( 'NONE', #9641, 1000.000000000000000 ) ;
#4920 = ORIENTED_EDGE ( 'NONE', *, *, #4739, .F. ) ;
#4921 = VECTOR ( 'NONE', #5665, 1000.000000000000000 ) ;
#4922 = CARTESIAN_POINT ( 'NONE',  ( -1.000896394980330006, -5.470974576271190770, 6.829956240957379521 ) ) ;
#4923 = CARTESIAN_POINT ( 'NONE',  ( 1.889999999999999902, 7.299999999999999822, -3.330669073875469621E-16 ) ) ;
#4924 = EDGE_CURVE ( 'NONE', #6699, #16493, #11985, .T. ) ;
#4925 = CARTESIAN_POINT ( 'NONE',  ( -1.401708661791369437, -1.241605122864669619, 6.590491606684078185 ) ) ;
#4926 = CARTESIAN_POINT ( 'NONE',  ( 1.661700935788380074, -5.337500000000000355, 3.038299064211610112 ) ) ;
#4927 = VECTOR ( 'NONE', #3346, 1000.000000000000000 ) ;
#4928 = PRESENTATION_LAYER_ASSIGNMENT (  '', '', ( #15623 ) ) ;
#4929 = ADVANCED_FACE ( 'NONE', ( #16066 ), #13111, .F. ) ;
#4930 = CARTESIAN_POINT ( 'NONE',  ( 2.642463257358089734, -4.148800282540726414, 4.945970783863369746 ) ) ;
#4931 = ORIENTED_EDGE ( 'NONE', *, *, #10489, .F. ) ;
#4932 = CARTESIAN_POINT ( 'NONE',  ( -1.458615186838411626, -5.103620102360555855, 3.259477383973569786 ) ) ;
#4933 = ADVANCED_FACE ( 'NONE', ( #684 ), #423, .T. ) ;
#4934 = CARTESIAN_POINT ( 'NONE',  ( 1.507201387236020151, -2.475884402143949892, 6.507509243627189299 ) ) ;
#4935 = ADVANCED_FACE ( 'NONE', ( #10590 ), #16244, .F. ) ;
#4936 = CIRCLE ( 'NONE', #15320, 0.5500000000000001554 ) ;
#4937 = FACE_OUTER_BOUND ( 'NONE', #16503, .T. ) ;
#4938 = VECTOR ( 'NONE', #152, 1000.000000000000000 ) ;
#4939 = CARTESIAN_POINT ( 'NONE',  ( -0.6628679656440360501, 3.050000000000000266, 1.670710678118650261 ) ) ;
#4940 = CARTESIAN_POINT ( 'NONE',  ( -0.7616804549307533145, -3.337551068810613142, 2.793499350326739350 ) ) ;
#4941 = LINE ( 'NONE', #11987, #14112 ) ;
#4942 = DIRECTION ( 'NONE',  ( -1.000000000000000000, -4.379659758543260954E-15, -5.767392335715200210E-18 ) ) ;
#4943 = CARTESIAN_POINT ( 'NONE',  ( -1.741179788930630190, -1.334758276017820267, 5.787747574231985936 ) ) ;
#4944 = ORIENTED_EDGE ( 'NONE', *, *, #10962, .T. ) ;
#4945 = LINE ( 'NONE', #2466, #1725 ) ;
#4946 = APPLICATION_CONTEXT ( 'automotive_design' ) ;
#4947 = VECTOR ( 'NONE', #6209, 1000.000000000000000 ) ;
#4948 = CARTESIAN_POINT ( 'NONE',  ( -0.009452110982655142699, -0.5998079552954631577, 2.050000000000001155 ) ) ;
#4949 = CARTESIAN_POINT ( 'NONE',  ( -1.771358649600341284, -1.264893411152960834, 6.676209054601235593 ) ) ;
#4950 = EDGE_LOOP ( 'NONE', ( #11583, #11150, #9356, #10286 ) ) ;
#4951 = PLANE ( 'NONE',  #4669 ) ;
#4952 = CARTESIAN_POINT ( 'NONE',  ( 1.936998685628529948, -0.8418633456037969420, 3.363294429306519895 ) ) ;
#4953 = LINE ( 'NONE', #10503, #7999 ) ;
#4954 = CARTESIAN_POINT ( 'NONE',  ( 1.949083719010301197, -5.059745762711855832, 4.055210292801453953 ) ) ;
#4955 = EDGE_LOOP ( 'NONE', ( #9507, #13430, #2038, #121 ) ) ;
#4956 = CIRCLE ( 'NONE', #15335, 0.1499999999999999667 ) ;
#4957 = VERTEX_POINT ( 'NONE', #1063 ) ;
#4958 = LINE ( 'NONE', #2286, #12744 ) ;
#4959 = CARTESIAN_POINT ( 'NONE',  ( -2.500000000000000000, -4.577131790655780032E-16, 4.000000000000000000 ) ) ;
#4960 = CARTESIAN_POINT ( 'NONE',  ( 0.9724415447670879953, -0.7068739681193980662, 2.553509270169310064 ) ) ;
#4961 = ADVANCED_FACE ( 'NONE', ( #15062 ), #14954, .T. ) ;
#4962 = EDGE_LOOP ( 'NONE', ( #16719, #10035, #17917, #17468 ) ) ;
#4963 = CARTESIAN_POINT ( 'NONE',  ( -1.647941990407690627, -5.555508474576275724, 3.475676388127094896 ) ) ;
#4964 = VECTOR ( 'NONE', #17473, 1000.000000000000000 ) ;
#4965 = CARTESIAN_POINT ( 'NONE',  ( -2.531332855772528756, -2.964938456198001671, 5.497162258444521221 ) ) ;
#4966 = CARTESIAN_POINT ( 'NONE',  ( -1.883442729065680776, -3.147403886144331420, 6.569694408006696129 ) ) ;
#4967 = VECTOR ( 'NONE', #7050, 1000.000000000000000 ) ;
#4968 = CARTESIAN_POINT ( 'NONE',  ( -1.889999999999999902, 4.700000000000000178, -6.736680183027569082E-16 ) ) ;
#4969 = DIRECTION ( 'NONE',  ( 0.000000000000000000, 0.000000000000000000, -1.000000000000000000 ) ) ;
#4970 = CARTESIAN_POINT ( 'NONE',  ( 2.353343516942209668, -3.826605122864669806, 4.722803042560139275 ) ) ;
#4971 = CARTESIAN_POINT ( 'NONE',  ( -1.899999999999999911, 4.218847493575600080E-16, -1.799976276337670169E-31 ) ) ;
#4972 = AXIS2_PLACEMENT_3D ( 'NONE', #12151, #9355, #12576 ) ;
#4973 = CARTESIAN_POINT ( 'NONE',  ( 2.500000000000000000, 4.700000000000000178, 0.6099999999999999867 ) ) ;
#4975 = EDGE_LOOP ( 'NONE', ( #16712, #12149, #4556, #15480 ) ) ;
#4974 = CARTESIAN_POINT ( 'NONE',  ( 0.5134687485628864900, -2.215872354612800521, 2.096259702418241222 ) ) ;
#4976 = CARTESIAN_POINT ( 'NONE',  ( -1.250000000000000000, 5.012741699796949391, 5.100000000000000533 ) ) ;
#4977 = DIRECTION ( 'NONE',  ( 1.142385477618690076E-14, -1.110223024625153952E-16, 1.000000000000000000 ) ) ;
#4978 = VECTOR ( 'NONE', #918, 1000.000000000000000 ) ;
#4979 = CARTESIAN_POINT ( 'NONE',  ( 1.794646911016580137, -1.167899381639829981, 6.222494056560660347 ) ) ;
#4980 = CARTESIAN_POINT ( 'NONE',  ( 1.549742865090599997, -0.4156779661016959948, 6.471102547561449647 ) ) ;
#4981 = VECTOR ( 'NONE', #16955, 1000.000000000000000 ) ;
#4982 = CARTESIAN_POINT ( 'NONE',  ( 1.149999999999999911, 9.299999999999998934, 7.599999999999999645 ) ) ;
#4983 = CARTESIAN_POINT ( 'NONE',  ( -0.4360591020458099987, -5.591101694915249887, 2.387347919655840034 ) ) ;
#4984 = ORIENTED_EDGE ( 'NONE', *, *, #10980, .T. ) ;
#4985 = DIRECTION ( 'NONE',  ( 1.000000000000000000, 0.000000000000000000, 0.000000000000000000 ) ) ;
#4986 = EDGE_CURVE ( 'NONE', #16040, #13169, #884, .T. ) ;
#4987 = ORIENTED_EDGE ( 'NONE', *, *, #6392, .F. ) ;
#4988 = CARTESIAN_POINT ( 'NONE',  ( 2.155845792290829177, -5.055296610169488503, 3.756158857535770945 ) ) ;
#4989 = CARTESIAN_POINT ( 'NONE',  ( 0.7500000000000000000, 6.450000000000000178, 3.200000000000000178 ) ) ;
#4990 = CARTESIAN_POINT ( 'NONE',  ( -1.889999999999999902, 7.299999999999999822, 0.6099999999999999867 ) ) ;
#4991 = ADVANCED_FACE ( 'NONE', ( #13660 ), #10782, .T. ) ;
#4992 =( GEOMETRIC_REPRESENTATION_CONTEXT ( 3 ) GLOBAL_UNCERTAINTY_ASSIGNED_CONTEXT ( ( #3983 ) ) GLOBAL_UNIT_ASSIGNED_CONTEXT ( ( #14596, #4773, #10424 ) ) REPRESENTATION_CONTEXT ( 'NONE', 'WORKASPACE' ) );
#4993 = VERTEX_POINT ( 'NONE', #12177 ) ;
#4994 = EDGE_LOOP ( 'NONE', ( #4297, #17280, #6359, #11695 ) ) ;
#4995 = CARTESIAN_POINT ( 'NONE',  ( 1.611907055891590002, -2.355602084342530045, 2.985210995296850189 ) ) ;
#4996 = DIRECTION ( 'NONE',  ( 1.054711873393900133E-14, 1.000000000000000000, 0.000000000000000000 ) ) ;
#4997 = DIRECTION ( 'NONE',  ( 1.000000000000000000, 0.000000000000000000, 0.000000000000000000 ) ) ;
#4998 = AXIS2_PLACEMENT_3D ( 'NONE', #11731, #17365, #10343 ) ;
#4999 = LINE ( 'NONE', #17558, #8759 ) ;
#5000 = EDGE_CURVE ( 'NONE', #14551, #11214, #6609, .T. ) ;
#5001 = CARTESIAN_POINT ( 'NONE',  ( 1.764807890102179977, -2.378890372630820149, 3.143016121304719857 ) ) ;
#5002 = CARTESIAN_POINT ( 'NONE',  ( 0.8189529353761060282, -3.822764246504690266, 2.493631540942729874 ) ) ;
#5003 = CARTESIAN_POINT ( 'NONE',  ( -0.3681613504765444134, -2.122719201459649874, 2.680257674196191431 ) ) ;
#5004 = FACE_OUTER_BOUND ( 'NONE', #517, .T. ) ;
#5005 = FACE_OUTER_BOUND ( 'NONE', #16882, .T. ) ;
#5006 = ORIENTED_EDGE ( 'NONE', *, *, #3031, .T. ) ;
#5007 = CARTESIAN_POINT ( 'NONE',  ( 1.899999999999999911, 2.799999999999999822, 1.600000000000000089 ) ) ;
#5008 = CARTESIAN_POINT ( 'NONE',  ( 0.8189529353761060282, -3.822764246504690266, 2.493631540942729874 ) ) ;
#5009 = ORIENTED_EDGE ( 'NONE', *, *, #15246, .F. ) ;
#5010 = AXIS2_PLACEMENT_3D ( 'NONE', #3157, #4626, #7509 ) ;
#5011 = ORIENTED_EDGE ( 'NONE', *, *, #3465, .F. ) ;
#5012 = DIRECTION ( 'NONE',  ( 3.097720492815730124E-16, 1.000000000000000000, 0.000000000000000000 ) ) ;
#5013 = EDGE_CURVE ( 'NONE', #11655, #1195, #6707, .T. ) ;
#5014 = EDGE_LOOP ( 'NONE', ( #15078, #7514, #15427, #17303, #10988, #1343, #7575, #7766 ) ) ;
#5015 = CARTESIAN_POINT ( 'NONE',  ( -0.1749999999999999889, 5.200000000000000178, 1.600000000000000089 ) ) ;
#5016 = APPLICATION_PROTOCOL_DEFINITION ( 'draft international standard', 'automotive_design', 1998, #2003 ) ;
#5017 = CARTESIAN_POINT ( 'NONE',  ( -1.610878918935079840, -5.268855932203385883, 2.590989782159090815 ) ) ;
#5018 = LINE ( 'NONE', #8087, #12025 ) ;
#5019 = AXIS2_PLACEMENT_3D ( 'NONE', #2673, #5538, #17002 ) ;
#5020 = CARTESIAN_POINT ( 'NONE',  ( -1.272929729338609262, -4.684430913171365063, 6.310761232086878003 ) ) ;
#5021 = CARTESIAN_POINT ( 'NONE',  ( -2.321479326063761395, -0.5491525423728815802, 3.414080590619972710 ) ) ;
#5022 = ORIENTED_EDGE ( 'NONE', *, *, #7232, .F. ) ;
#5023 = CARTESIAN_POINT ( 'NONE',  ( 2.116444151961470066, -0.05338983050847490031, 3.670839500609349937 ) ) ;
#5024 = ORIENTED_EDGE ( 'NONE', *, *, #2120, .T. ) ;
#5025 = DIRECTION ( 'NONE',  ( 0.000000000000000000, 0.000000000000000000, 1.000000000000000000 ) ) ;
#5026 = DIRECTION ( 'NONE',  ( 0.000000000000000000, 0.000000000000000000, 1.000000000000000000 ) ) ;
#5027 = CARTESIAN_POINT ( 'NONE',  ( -0.03000000000000050196, 11.40000000000000036, 1.600000000000000089 ) ) ;
#5028 = CIRCLE ( 'NONE', #317, 1.016666666666670160 ) ;
#5029 = CARTESIAN_POINT ( 'NONE',  ( 2.350067830300900162, -5.377542372881360500, 4.825253242917690422 ) ) ;
#5030 = CARTESIAN_POINT ( 'NONE',  ( -2.051568858000911266, -5.080331814072260421, 3.016498023208352919 ) ) ;
#5031 = VERTEX_POINT ( 'NONE', #12454 ) ;
#5032 = LINE ( 'NONE', #6409, #16724 ) ;
#5033 = CARTESIAN_POINT ( 'NONE',  ( 1.802718065953961002, -0.5662447625043125488, 3.717600174934180046 ) ) ;
#5034 = CARTESIAN_POINT ( 'NONE',  ( -2.524473153133541814, -4.987178660919110662, 3.881373716577405819 ) ) ;
#5035 = CARTESIAN_POINT ( 'NONE',  ( -1.599999999999880185, 11.40000000000000036, -2.399999999999999911 ) ) ;
#5036 = FACE_OUTER_BOUND ( 'NONE', #6640, .T. ) ;
#5037 = CARTESIAN_POINT ( 'NONE',  ( 1.823404397755048700, -3.943046564306109669, 5.643450181448720571 ) ) ;
#5038 = FACE_OUTER_BOUND ( 'NONE', #132, .T. ) ;
#5039 = DIRECTION ( 'NONE',  ( -4.377285571048150598E-15, 1.000000000000000000, 0.000000000000000000 ) ) ;
#5040 = CARTESIAN_POINT ( 'NONE',  ( -1.974086094277271108, -1.404623140882690580, 5.263813741415750869 ) ) ;
#5041 = ORIENTED_EDGE ( 'NONE', *, *, #12544, .F. ) ;
#5042 = DIRECTION ( 'NONE',  ( 1.000000000000000000, 0.000000000000000000, 0.000000000000000000 ) ) ;
#5043 = VECTOR ( 'NONE', #8866, 1000.000000000000000 ) ;
#5044 = CARTESIAN_POINT ( 'NONE',  ( 1.899999999999999911, 0.7500000000000000000, 7.649999999999999467 ) ) ;
#5045 = ADVANCED_FACE ( 'NONE', ( #4012 ), #3925, .T. ) ;
#5046 = CARTESIAN_POINT ( 'NONE',  ( -0.009452110982655128821, -0.5998079552954630467, 2.350000000000000089 ) ) ;
#5047 = CARTESIAN_POINT ( 'NONE',  ( -2.531332855772528756, -2.964938456198001671, 5.497162258444521221 ) ) ;
#5048 = EDGE_CURVE ( 'NONE', #15121, #747, #6143, .T. ) ;
#5049 = ORIENTED_EDGE ( 'NONE', *, *, #14959, .F. ) ;
#5050 = DIRECTION ( 'NONE',  ( -1.908195823574489776E-16, 1.000000000000000000, 0.000000000000000000 ) ) ;
#5051 = CARTESIAN_POINT ( 'NONE',  ( 1.480680413335799805, -1.214475958216410190, 6.529298007719799735 ) ) ;
#5052 = DIRECTION ( 'NONE',  ( 0.000000000000000000, 0.000000000000000000, 1.000000000000000000 ) ) ;
#5053 = CARTESIAN_POINT ( 'NONE',  ( 0.4974685680287860290, -5.139830508474580562, 7.000224381598740386 ) ) ;
#5054 = EDGE_LOOP ( 'NONE', ( #2880, #1928, #10963, #11973 ) ) ;
#5055 = EDGE_LOOP ( 'NONE', ( #11550, #10659, #7515, #6788 ) ) ;
#5056 = LINE ( 'NONE', #989, #16585 ) ;
#5057 = CARTESIAN_POINT ( 'NONE',  ( -9.552245033349350628E-16, 7.799999999999999822, 4.776122516674680244E-16 ) ) ;
#5058 = DIRECTION ( 'NONE',  ( 1.000000000000000000, 0.000000000000000000, 0.000000000000000000 ) ) ;
#5059 = ORIENTED_EDGE ( 'NONE', *, *, #15508, .F. ) ;
#5060 = CARTESIAN_POINT ( 'NONE',  ( 2.030998484741458832, -5.381991525423726053, 4.999543428097175557 ) ) ;
#5061 = CARTESIAN_POINT ( 'NONE',  ( -2.567863625471609179, -3.104668185927728974, 4.029783546918099368 ) ) ;
#5062 = DIRECTION ( 'NONE',  ( 1.000000000000000000, -1.059690869644410208E-14, 0.000000000000000000 ) ) ;
#5063 = LINE ( 'NONE', #3483, #1136 ) ;
#5064 = CARTESIAN_POINT ( 'NONE',  ( 0.02999999999999850009, 12.00000000000000000, 7.649999999999999467 ) ) ;
#5065 = CARTESIAN_POINT ( 'NONE',  ( -1.902324933209429858, -3.197821339080880065, 3.314393441133570040 ) ) ;
#5066 = CARTESIAN_POINT ( 'NONE',  ( -1.500000000000000000, -5.599999999999999645, 2.299999999999999822 ) ) ;
#5067 = FACE_OUTER_BOUND ( 'NONE', #8819, .T. ) ;
#5069 = EDGE_LOOP ( 'NONE', ( #6880, #1766, #3565, #14702 ) ) ;
#5068 = CARTESIAN_POINT ( 'NONE',  ( 1.213493134184789657, -2.285737219477670390, 2.339799138571409642 ) ) ;
#5070 = CARTESIAN_POINT ( 'NONE',  ( 0.5372984490435490645, 4.599999999999999645, 7.700000000000000178 ) ) ;
#5071 = EDGE_CURVE ( 'NONE', #6378, #4752, #2461, .T. ) ;
#5072 = LINE ( 'NONE', #14992, #7068 ) ;
#5073 = LINE ( 'NONE', #11929, #13514 ) ;
#5074 = EDGE_CURVE ( 'NONE', #16255, #5452, #16531, .T. ) ;
#5075 = CARTESIAN_POINT ( 'NONE',  ( -2.111627294540180166, -1.889836318576769925, 3.660877362176710559 ) ) ;
#5076 = CARTESIAN_POINT ( 'NONE',  ( 0.002826310976695059745, -5.105205364259369993, 2.204978094066150085 ) ) ;
#5077 = CARTESIAN_POINT ( 'NONE',  ( -0.5500000000000000444, 6.450000000000000178, 3.600000000000000089 ) ) ;
#5078 = CARTESIAN_POINT ( 'NONE',  ( -1.194742379459959869, -5.475423728813559876, 6.727584234649759409 ) ) ;
#5079 = ORIENTED_EDGE ( 'NONE', *, *, #7667, .F. ) ;
#5080 = ORIENTED_EDGE ( 'NONE', *, *, #6179, .F. ) ;
#5081 = CARTESIAN_POINT ( 'NONE',  ( 1.811729841638689775, -5.041949152542367862, 3.197954009834290456 ) ) ;
#5082 = DIRECTION ( 'NONE',  ( 1.000000000000000000, -3.700743415417190112E-16, 0.000000000000000000 ) ) ;
#5083 = DIRECTION ( 'NONE',  ( 1.000000000000000000, 0.000000000000000000, 0.000000000000000000 ) ) ;
#5084 = ORIENTED_EDGE ( 'NONE', *, *, #7259, .T. ) ;
#5085 = EDGE_CURVE ( 'NONE', #6674, #4421, #15150, .T. ) ;
#5086 = CARTESIAN_POINT ( 'NONE',  ( 0.5570002967656469961, -2.891232714973159812, 6.986590552960210587 ) ) ;
#5087 = CARTESIAN_POINT ( 'NONE',  ( -0.5500000000000000444, 7.799999999999999822, 1.600000000000000089 ) ) ;
#5088 = CARTESIAN_POINT ( 'NONE',  ( -3.766169468773179610E-15, -5.599999999999999645, 2.349999999999999645 ) ) ;
#5089 = CARTESIAN_POINT ( 'NONE',  ( 0.5000000000000000000, 5.762741699796949391, 6.100000000000000533 ) ) ;
#5090 = CARTESIAN_POINT ( 'NONE',  ( 1.611907055891590002, -2.355602084342530045, 2.985210995296850189 ) ) ;
#5091 = CARTESIAN_POINT ( 'NONE',  ( -2.239137794397029868, -4.987178660919110662, 3.975425900939220103 ) ) ;
#5092 = CARTESIAN_POINT ( 'NONE',  ( 0.9742769543504904428, -1.261052534792989288, 6.507120986223561054 ) ) ;
#5093 = EDGE_CURVE ( 'NONE', #6773, #2121, #11055, .T. ) ;
#5094 = CARTESIAN_POINT ( 'NONE',  ( 0.1565249325564390115, -0.4468220338983060480, 7.048192310558509810 ) ) ;
#5095 = CARTESIAN_POINT ( 'NONE',  ( -0.1869574461324000070, -0.5962015548080630278, 2.350675676344399889 ) ) ;
#5096 = ORIENTED_EDGE ( 'NONE', *, *, #2841, .F. ) ;
#5097 = DIRECTION ( 'NONE',  ( -1.000000000000000000, -1.908195823574489776E-16, -1.110223024625159992E-16 ) ) ;
#5098 = CARTESIAN_POINT ( 'NONE',  ( -1.699999999999999956, 2.299999999999999822, 7.700000000000000178 ) ) ;
#5099 = AXIS2_PLACEMENT_3D ( 'NONE', #14607, #10698, #1758 ) ;
#5100 = CARTESIAN_POINT ( 'NONE',  ( 1.571912189623089873, -4.335106588847041031, 6.451524409078630562 ) ) ;
#5101 = ORIENTED_EDGE ( 'NONE', *, *, #4739, .T. ) ;
#5102 = ORIENTED_EDGE ( 'NONE', *, *, #13168, .T. ) ;
#5103 = CARTESIAN_POINT ( 'NONE',  ( 1.750000000000000000, 11.40000000000000036, 7.550000000000000711 ) ) ;
#5104 = EDGE_LOOP ( 'NONE', ( #4680, #9353, #4000, #3471 ) ) ;
#5105 = CARTESIAN_POINT ( 'NONE',  ( 1.399999999999999911, -8.000000000000000000, 3.299999999999999822 ) ) ;
#5106 = APPLICATION_PROTOCOL_DEFINITION ( 'draft international standard', 'automotive_design', 1998, #4249 ) ;
#5107 = CARTESIAN_POINT ( 'NONE',  ( -1.978267656359410154, -5.197669491525420682, 5.974740860598790171 ) ) ;
#5108 = EDGE_CURVE ( 'NONE', #4535, #6313, #10976, .T. ) ;
#5109 = LINE ( 'NONE', #13726, #1444 ) ;
#5110 = ORIENTED_EDGE ( 'NONE', *, *, #13568, .F. ) ;
#5111 = CARTESIAN_POINT ( 'NONE',  ( 2.296954468777709923, -0.6361096273691760894, 4.187412587068650716 ) ) ;
#5112 = LINE ( 'NONE', #18132, #15622 ) ;
#5113 = CARTESIAN_POINT ( 'NONE',  ( 2.053221424930760097, -0.8651516338920849369, 3.549770689668250157 ) ) ;
#5114 = CARTESIAN_POINT ( 'NONE',  ( -0.3171869470818471370, -0.1557203389830511819, 7.334814496515233095 ) ) ;
#5115 = EDGE_CURVE ( 'NONE', #14832, #9752, #6893, .T. ) ;
#5116 =( BOUNDED_CURVE ( )  B_SPLINE_CURVE ( 3, ( #10259, #14613, #16022, #9044 ),
 .UNSPECIFIED., .F., .F. ) 
 B_SPLINE_CURVE_WITH_KNOTS ( ( 4, 4 ),
 ( 0.000000000000000000, 1.000000000000000000 ),
 .UNSPECIFIED. ) 
 CURVE ( )  GEOMETRIC_REPRESENTATION_ITEM ( )  RATIONAL_B_SPLINE_CURVE ( ( 1.000000000000000000, 0.8047378541243649375, 0.8047378541243649375, 1.000000000000000000 ) ) 
 REPRESENTATION_ITEM ( '' )  );
#5117 = VERTEX_POINT ( 'NONE', #6807 ) ;
#5118 = CARTESIAN_POINT ( 'NONE',  ( 0.4360591020457930123, -0.3088983050847460277, 2.387347919655840034 ) ) ;
#5119 = CARTESIAN_POINT ( 'NONE',  ( -2.020286629067959971, -0.1913135593220339215, 6.420841923842841581 ) ) ;
#5120 = ORIENTED_EDGE ( 'NONE', *, *, #582, .T. ) ;
#5121 = CARTESIAN_POINT ( 'NONE',  ( 0.7093417302541469294, -5.435381355932199732, 6.943956659919690466 ) ) ;
#5122 = AXIS2_PLACEMENT_3D ( 'NONE', #3210, #15901, #15999 ) ;
#5123 = CARTESIAN_POINT ( 'NONE',  ( 2.033393610350128888, -0.8224159336754828242, 5.884928737465322079 ) ) ;
#5124 = CARTESIAN_POINT ( 'NONE',  ( -0.009452110982655715157, -0.5998079552954631577, 2.649999999999998579 ) ) ;
#5125 = CARTESIAN_POINT ( 'NONE',  ( 1.008962495263989956, -0.9854339516935015642, 7.154609617872576877 ) ) ;
#5126 = ORIENTED_EDGE ( 'NONE', *, *, #17463, .F. ) ;
#5127 = CARTESIAN_POINT ( 'NONE',  ( -0.7252674547190166576, -5.211074464177385401, 2.776474344060209987 ) ) ;
#5128 = CARTESIAN_POINT ( 'NONE',  ( -1.115198193348240219, -4.338947465207009913, 6.772457159276569882 ) ) ;
#5129 = CARTESIAN_POINT ( 'NONE',  ( -2.501774541437291610, -4.824160642901089702, 5.585572039315926496 ) ) ;
#5130 = DIRECTION ( 'NONE',  ( -2.529805069132844337E-15, 1.000000000000000000, 1.807003620809174385E-16 ) ) ;
#5131 = CARTESIAN_POINT ( 'NONE',  ( -2.500000000000000000, 5.551115123125779744E-16, -1.799976276337670169E-31 ) ) ;
#5132 = CARTESIAN_POINT ( 'NONE',  ( -1.928470600873600782, -3.127956474216021299, 3.995796205495660391 ) ) ;
#5133 = CARTESIAN_POINT ( 'NONE',  ( -1.899999999999999911, 2.799999999999999822, 0.5999999999999999778 ) ) ;
#5134 = DIRECTION ( 'NONE',  ( -1.000000000000000000, 2.891205793294678228E-15, 3.614007241618347587E-15 ) ) ;
#5135 = CARTESIAN_POINT ( 'NONE',  ( -0.3509990757148119811, -1.125163681423229756, 6.722795464567655976 ) ) ;
#5136 = ORIENTED_EDGE ( 'NONE', *, *, #5197, .T. ) ;
#5137 = CARTESIAN_POINT ( 'NONE',  ( 0.1749999999999999889, 6.799999999999999822, 1.600000000000000089 ) ) ;
#5138 = CYLINDRICAL_SURFACE ( 'NONE', #17375, 0.01000000000000002623 ) ;
#5139 = CARTESIAN_POINT ( 'NONE',  ( 0.2751970330256541808, -0.3251990024832501214, 2.050771348498781066 ) ) ;
#5140 = CARTESIAN_POINT ( 'NONE',  ( 0.5385843327681005821, -1.916965483225031130, 2.101338688959521139 ) ) ;
#5141 = ORIENTED_EDGE ( 'NONE', *, *, #760, .F. ) ;
#5142 = LINE ( 'NONE', #17612, #1104 ) ;
#5143 = FACE_OUTER_BOUND ( 'NONE', #2218, .T. ) ;
#5144 = CARTESIAN_POINT ( 'NONE',  ( 1.679950111053631900, -5.104237288135595740, 5.880020650119711867 ) ) ;
#5145 = ORIENTED_EDGE ( 'NONE', *, *, #7216, .F. ) ;
#5146 = ORIENTED_EDGE ( 'NONE', *, *, #4829, .T. ) ;
#5147 = CARTESIAN_POINT ( 'NONE',  ( 1.399999999999999911, 0.5999999999999999778, 3.299999999999999822 ) ) ;
#5148 = PLANE ( 'NONE',  #8518 ) ;
#5149 = FACE_OUTER_BOUND ( 'NONE', #16926, .T. ) ;
#5150 = VERTEX_POINT ( 'NONE', #16702 ) ;
#5151 = CARTESIAN_POINT ( 'NONE',  ( 1.713314936023349944, -5.338983050847460277, 3.089913064446569546 ) ) ;
#5152 = CARTESIAN_POINT ( 'NONE',  ( -1.256119432346030962, -4.338947465207014353, 7.037793332329566276 ) ) ;
#5153 = PLANE ( 'NONE',  #15959 ) ;
#5154 = CARTESIAN_POINT ( 'NONE',  ( 1.208047591394629925E-13, 11.40000000000000036, -5.003920418925160367E-17 ) ) ;
#5155 = DIRECTION ( 'NONE',  ( 1.000000000000000000, 8.074349270001130318E-16, 0.000000000000000000 ) ) ;
#5156 = EDGE_CURVE ( 'NONE', #18019, #490, #13933, .T. ) ;
#5157 = CARTESIAN_POINT ( 'NONE',  ( 2.091095264232530226, -3.943046564306110113, 5.779845490516200002 ) ) ;
#5158 = DIRECTION ( 'NONE',  ( 2.220446049250309876E-16, 1.000000000000000000, -1.268826313857319964E-16 ) ) ;
#5159 = CARTESIAN_POINT ( 'NONE',  ( 1.000000000000000000, -5.500000000000000000, 5.100000000000000533 ) ) ;
#5160 = CARTESIAN_POINT ( 'NONE',  ( -1.392767620582729293, -2.029566048306499670, 2.440948861123721780 ) ) ;
#5161 = CARTESIAN_POINT ( 'NONE',  ( 0.1749999999999999889, 7.700000000000000178, 1.600000000000000089 ) ) ;
#5162 = CARTESIAN_POINT ( 'NONE',  ( 1.596341326794969984, -0.3355932203389830337, 2.970780074643809776 ) ) ;
#5163 = CARTESIAN_POINT ( 'NONE',  ( 1.902324933209389890, -2.402178660919109809, 3.314393441133530072 ) ) ;
#5164 = CARTESIAN_POINT ( 'NONE',  ( 1.399999999999999911, -7.000000000000000000, 6.100000000000000533 ) ) ;
#5165 = PLANE ( 'NONE',  #7988 ) ;
#5166 = CARTESIAN_POINT ( 'NONE',  ( -1.428515267734880023, -5.568855932203390147, 2.829745655876930055 ) ) ;
#5167 = VERTEX_POINT ( 'NONE', #15610 ) ;
#5168 = EDGE_CURVE ( 'NONE', #4341, #4730, #6982, .T. ) ;
#5169 = FILL_AREA_STYLE_COLOUR ( '', #13434 ) ;
#5170 = VERTEX_POINT ( 'NONE', #10045 ) ;
#5171 = CARTESIAN_POINT ( 'NONE',  ( -0.1565249325564299632, -5.153177966101688767, 7.048192310558507145 ) ) ;
#5172 = DIRECTION ( 'NONE',  ( 0.000000000000000000, 1.359631073446889961E-32, -1.000000000000000000 ) ) ;
#5173 = DIRECTION ( 'NONE',  ( 1.233581138472399909E-16, -5.135813185032649012E-32, 1.000000000000000000 ) ) ;
#5174 = EDGE_CURVE ( 'NONE', #4443, #14407, #9539, .T. ) ;
#5175 = ORIENTED_EDGE ( 'NONE', *, *, #17723, .T. ) ;
#5176 = CARTESIAN_POINT ( 'NONE',  ( 2.192143888961729736, -4.218665147405599392, 5.556300681753580051 ) ) ;
#5177 = EDGE_CURVE ( 'NONE', #5929, #3082, #7182, .T. ) ;
#5178 = CARTESIAN_POINT ( 'NONE',  ( -1.899999999999999911, 4.700000000000000178, 0.5999999999999999778 ) ) ;
#5179 = CARTESIAN_POINT ( 'NONE',  ( 2.043308330018790198, -5.399788135593220240, 5.867646457774659652 ) ) ;
#5180 = EDGE_CURVE ( 'NONE', #5374, #12675, #7359, .T. ) ;
#5181 = CARTESIAN_POINT ( 'NONE',  ( 0.9000000000000000222, 6.450000000000000178, 3.600000000000000089 ) ) ;
#5182 = EDGE_CURVE ( 'NONE', #16755, #18019, #8423, .T. ) ;
#5183 = DIRECTION ( 'NONE',  ( -1.233581138472399909E-16, 1.000000000000000000, 0.000000000000000000 ) ) ;
#5184 = CARTESIAN_POINT ( 'NONE',  ( 0.4539185741479240255, -2.215872354612800521, 2.390735265170440105 ) ) ;
#5185 = VECTOR ( 'NONE', #13283, 1000.000000000000000 ) ;
#5186 = CARTESIAN_POINT ( 'NONE',  ( 0.009452039534068971960, -5.000193177104105047, 2.350000000173209536 ) ) ;
#5187 = CARTESIAN_POINT ( 'NONE',  ( -1.203420131881960398, -1.540511994252448780, 6.363334551077827861 ) ) ;
#5188 = DIRECTION ( 'NONE',  ( -0.000000000000000000, 1.000000000000000000, 0.000000000000000000 ) ) ;
#5189 = CARTESIAN_POINT ( 'NONE',  ( 0.009452110982654783611, -0.3001920447045380858, 2.050000000000001155 ) ) ;
#5190 = EDGE_LOOP ( 'NONE', ( #11215, #17233, #12358, #17522 ) ) ;
#5191 = LINE ( 'NONE', #3415, #15640 ) ;
#5192 = CARTESIAN_POINT ( 'NONE',  ( 3.673940397442067510E-17, 2.600000000000000089, 7.750000000000000000 ) ) ;
#5193 = CARTESIAN_POINT ( 'NONE',  ( -2.349129089426440054, -4.894025507765950245, 4.842612091679129982 ) ) ;
#5194 = ORIENTED_EDGE ( 'NONE', *, *, #9614, .F. ) ;
#5195 = VERTEX_POINT ( 'NONE', #14298 ) ;
#5196 = CARTESIAN_POINT ( 'NONE',  ( 0.1749999999999999889, 7.500000000000000000, 3.100000000000000089 ) ) ;
#5197 = EDGE_CURVE ( 'NONE', #6584, #2212, #2738, .T. ) ;
#5198 = ORIENTED_EDGE ( 'NONE', *, *, #13042, .F. ) ;
#5199 = DIRECTION ( 'NONE',  ( 7.930164461608259947E-17, 0.000000000000000000, 1.000000000000000000 ) ) ;
#5200 = CARTESIAN_POINT ( 'NONE',  ( -0.5889081234606770021, -5.162076271186439413, 6.978529000034869867 ) ) ;
#5201 = EDGE_CURVE ( 'NONE', #1517, #9915, #8468, .T. ) ;
#5202 = ORIENTED_EDGE ( 'NONE', *, *, #16644, .T. ) ;
#5203 =( REPRESENTATION_RELATIONSHIP ('NONE','NONE', #2757, #853 ) REPRESENTATION_RELATIONSHIP_WITH_TRANSFORMATION ( #11959 )SHAPE_REPRESENTATION_RELATIONSHIP( ) );
#5204 = AXIS2_PLACEMENT_3D ( 'NONE', #4243, #15744, #9815 ) ;
#5205 = CARTESIAN_POINT ( 'NONE',  ( -1.401708661791369881, -1.241605122864670063, 6.590491606684079962 ) ) ;
#5206 = DIRECTION ( 'NONE',  ( 0.000000000000000000, 0.000000000000000000, 1.000000000000000000 ) ) ;
#5207 = AXIS2_PLACEMENT_3D ( 'NONE', #3792, #14912, #14816 ) ;
#5208 = CARTESIAN_POINT ( 'NONE',  ( 1.936998685628529948, -0.8418633456037969420, 3.363294429306519895 ) ) ;
#5209 = CARTESIAN_POINT ( 'NONE',  ( 2.011500846714319835, -0.04894067796610199889, 3.478373409938460448 ) ) ;
#5210 = ORIENTED_EDGE ( 'NONE', *, *, #6782, .F. ) ;
#5211 = CARTESIAN_POINT ( 'NONE',  ( 1.850000000000000089, 0.7500000000000000000, 8.300000000000000711 ) ) ;
#5212 = DIRECTION ( 'NONE',  ( 0.000000000000000000, 3.548581835996780230E-45, -1.000000000000000000 ) ) ;
#5213 = AXIS2_PLACEMENT_3D ( 'NONE', #13567, #9291, #4844 ) ;
#5214 = CARTESIAN_POINT ( 'NONE',  ( -2.311987889326990064, -1.521064582324129777, 4.260161748947140836 ) ) ;
#5215 = FACE_OUTER_BOUND ( 'NONE', #14266, .T. ) ;
#5216 = CARTESIAN_POINT ( 'NONE',  ( -1.771358649600341284, -1.264893411152960834, 6.676209054601235593 ) ) ;
#5217 = EDGE_CURVE ( 'NONE', #18244, #13417, #14018, .T. ) ;
#5218 = EDGE_LOOP ( 'NONE', ( #4491, #13445, #4189, #2909 ) ) ;
#5219 = FACE_OUTER_BOUND ( 'NONE', #13671, .T. ) ;
#5220 = CARTESIAN_POINT ( 'NONE',  ( 1.710920205120059823, -4.012911429170970656, 6.316012914303540171 ) ) ;
#5221 = CARTESIAN_POINT ( 'NONE',  ( -1.233489123281609645, -4.637854336594775084, 7.049812391606588236 ) ) ;
#5222 = DIRECTION ( 'NONE',  ( 1.899065700016719806E-16, 1.000000000000000000, 0.000000000000000000 ) ) ;
#5223 = DIRECTION ( 'NONE',  ( 1.445602896647339508E-15, 0.000000000000000000, 1.000000000000000000 ) ) ;
#5224 = VECTOR ( 'NONE', #16030, 1000.000000000000000 ) ;
#5225 = CARTESIAN_POINT ( 'NONE',  ( -1.996236309555629251, -4.548542059801595094, 5.179523137126564869 ) ) ;
#5226 = CARTESIAN_POINT ( 'NONE',  ( 1.000000000000000000, -6.000000000000000000, 5.100000000000000533 ) ) ;
#5227 = CARTESIAN_POINT ( 'NONE',  ( -0.5500000000000000444, 6.450000000000000178, 3.200000000000000178 ) ) ;
#5228 = AXIS2_PLACEMENT_3D ( 'NONE', #2686, #1574, #4431 ) ;
#5229 = CARTESIAN_POINT ( 'NONE',  ( -0.01333550863832440661, -3.430704221963769562, 2.647020699851690306 ) ) ;
#5230 = ORIENTED_EDGE ( 'NONE', *, *, #15207, .F. ) ;
#5231 = DIRECTION ( 'NONE',  ( 1.823160359065819982E-16, 0.000000000000000000, -1.000000000000000000 ) ) ;
#5232 = VECTOR ( 'NONE', #17268, 1000.000000000000000 ) ;
#5233 = CARTESIAN_POINT ( 'NONE',  ( 0.5999999999999999778, 10.80000000000000071, 7.700000000000000178 ) ) ;
#5234 = CARTESIAN_POINT ( 'NONE',  ( -1.869504824896970119, -0.2046610169491529518, 5.548311746956866131 ) ) ;
#5235 = CARTESIAN_POINT ( 'NONE',  ( 1.349044826018420906, -0.4774152569121725143, 3.148480103883603221 ) ) ;
#5236 = CARTESIAN_POINT ( 'NONE',  ( -2.647661051184980519, -3.058091609351150986, 4.518328177639144627 ) ) ;
#5237 = FACE_BOUND ( 'NONE', #12867, .T. ) ;
#5238 = VECTOR ( 'NONE', #9468, 1000.000000000000000 ) ;
#5239 = VECTOR ( 'NONE', #17161, 1000.000000000000000 ) ;
#5240 = DIRECTION ( 'NONE',  ( 1.224646799147350002E-16, -1.000000000000000000, -6.123233995736769734E-17 ) ) ;
#5241 = CARTESIAN_POINT ( 'NONE',  ( -1.647941990407690627, -5.255508474576275901, 3.475676388127094896 ) ) ;
#5242 = VERTEX_POINT ( 'NONE', #12630 ) ;
#5243 = VERTEX_POINT ( 'NONE', #18257 ) ;
#5244 = DIRECTION ( 'NONE',  ( 1.000000000000000000, 0.000000000000000000, 0.000000000000000000 ) ) ;
#5245 = DIRECTION ( 'NONE',  ( 0.000000000000000000, 0.000000000000000000, -1.000000000000000000 ) ) ;
#5246 = DIRECTION ( 'NONE',  ( 1.000000000000000000, 1.168655815394900078E-16, 2.220446049250309876E-16 ) ) ;
#5247 = ORIENTED_EDGE ( 'NONE', *, *, #540, .T. ) ;
#5248 = VECTOR ( 'NONE', #12457, 1000.000000000000000 ) ;
#5249 = CARTESIAN_POINT ( 'NONE',  ( -2.253200202764409799, -5.511016949152540256, 5.379408587037509903 ) ) ;
#5250 = AXIS2_PLACEMENT_3D ( 'NONE', #361, #4779, #11555 ) ;
#5251 = CARTESIAN_POINT ( 'NONE',  ( -2.629224451638860760, -4.641695212954759064, 4.339039509243916015 ) ) ;
#5252 = DIRECTION ( 'NONE',  ( 2.220446049250309876E-16, 1.000000000000000000, 0.000000000000000000 ) ) ;
#5253 = CARTESIAN_POINT ( 'NONE',  ( -1.236224677598320332, -3.613169651910099756, 2.351625617688101411 ) ) ;
#5254 = DIRECTION ( 'NONE',  ( -1.224646799147341867E-16, -1.000000000000000000, 0.000000000000000000 ) ) ;
#5255 = AXIS2_PLACEMENT_3D ( 'NONE', #11225, #4087, #16869 ) ;
#5256 = CARTESIAN_POINT ( 'NONE',  ( 0.7778405029480717214, -0.9854339516935015642, 6.599964735094206780 ) ) ;
#5257 = VECTOR ( 'NONE', #12708, 1000.000000000000000 ) ;
#5258 = VECTOR ( 'NONE', #17401, 1000.000000000000000 ) ;
#5259 = FACE_OUTER_BOUND ( 'NONE', #3499, .T. ) ;
#5260 = DIRECTION ( 'NONE',  ( 0.000000000000000000, 1.110223024625159992E-16, -1.000000000000000000 ) ) ;
#5262 = VERTEX_POINT ( 'NONE', #11518 ) ;
#5261 = CARTESIAN_POINT ( 'NONE',  ( 0.1366863161731129428, -2.937809291549738688, 7.350364228549148393 ) ) ;
#5263 = AXIS2_PLACEMENT_3D ( 'NONE', #14963, #1070, #7824 ) ;
#5264 = CARTESIAN_POINT ( 'NONE',  ( -1.000000000000000000, 5.799999999999999822, 7.700000000000000178 ) ) ;
#5265 = CARTESIAN_POINT ( 'NONE',  ( -2.351526912647309953, -0.5269067796610169552, 4.606040641882809261 ) ) ;
#5266 = CARTESIAN_POINT ( 'NONE',  ( 1.707817112497189926, -0.4112288135593229477, 6.319218296629480314 ) ) ;
#5267 = CARTESIAN_POINT ( 'NONE',  ( 0.2365712905368450025, -2.192584066324519743, 2.358466376073659720 ) ) ;
#5268 = CARTESIAN_POINT ( 'NONE',  ( 0.009452039534068971960, -5.000193177104105047, 2.350000000173209536 ) ) ;
#5269 = DIRECTION ( 'NONE',  ( 0.000000000000000000, 0.000000000000000000, -1.000000000000000000 ) ) ;
#5270 = CARTESIAN_POINT ( 'NONE',  ( -1.973760952634090238, -5.559957627118640389, 2.925986839873730982 ) ) ;
#5271 = ORIENTED_EDGE ( 'NONE', *, *, #17952, .F. ) ;
#5272 = DIRECTION ( 'NONE',  ( 0.000000000000000000, -1.000000000000000000, 8.673617379884027583E-16 ) ) ;
#5273 = EDGE_LOOP ( 'NONE', ( #2821, #10735, #18043, #8829, #13549, #17565, #2677, #2846, #7741, #4236, #16037, #11143, #16726, #18151, #3342, #12368 ) ) ;
#5274 = FACE_OUTER_BOUND ( 'NONE', #12442, .T. ) ;
#5275 = LINE ( 'NONE', #5455, #14735 ) ;
#5276 = VECTOR ( 'NONE', #16361, 1000.000000000000000 ) ;
#5277 = VECTOR ( 'NONE', #6291, 1000.000000000000000 ) ;
#5278 = ORIENTED_EDGE ( 'NONE', *, *, #17844, .T. ) ;
#5279 = CARTESIAN_POINT ( 'NONE',  ( -1.465095039565370127, -3.566593075333519991, 2.858195935359880480 ) ) ;
#5280 = VECTOR ( 'NONE', #7789, 1000.000000000000000 ) ;
#5281 = CARTESIAN_POINT ( 'NONE',  ( -2.306642602145299925, -5.515466101694909362, 5.166805192608490138 ) ) ;
#5282 = FACE_OUTER_BOUND ( 'NONE', #8334, .T. ) ;
#5283 = DIRECTION ( 'NONE',  ( 0.000000000000000000, 1.000000000000000000, 0.000000000000000000 ) ) ;
#5284 = CARTESIAN_POINT ( 'NONE',  ( 2.322440385110930094, -2.518620102360550117, 4.319189883157390497 ) ) ;
#5285 = VECTOR ( 'NONE', #515, 1000.000000000000000 ) ;
#5286 = CYLINDRICAL_SURFACE ( 'NONE', #12606, 0.6000000000000000888 ) ;
#5287 = VECTOR ( 'NONE', #7769, 1000.000000000000000 ) ;
#5288 = CARTESIAN_POINT ( 'NONE',  ( 1.712910428781929006, -2.704926408666860738, 5.831741890007691609 ) ) ;
#5289 = DIRECTION ( 'NONE',  ( 3.315303352997239924E-31, -1.000000000000000000, 8.588360937600549480E-46 ) ) ;
#5290 = CARTESIAN_POINT ( 'NONE',  ( 7.233457020361919865E-16, 4.000000000000000000, 5.100000000000000533 ) ) ;
#5291 = ORIENTED_EDGE ( 'NONE', *, *, #1518, .T. ) ;
#5292 = EDGE_CURVE ( 'NONE', #14118, #3787, #11760, .T. ) ;
#5293 = DIRECTION ( 'NONE',  ( 0.7071067811865480168, 0.7071067811865470176, 0.000000000000000000 ) ) ;
#5294 = CARTESIAN_POINT ( 'NONE',  ( 1.250000000000000000, 7.799999999999999822, 6.100000000000000533 ) ) ;
#5295 = VERTEX_POINT ( 'NONE', #16893 ) ;
#5296 = EDGE_CURVE ( 'NONE', #8570, #10292, #4200, .T. ) ;
#5297 = ORIENTED_EDGE ( 'NONE', *, *, #9111, .F. ) ;
#5298 = EDGE_CURVE ( 'NONE', #9985, #2611, #15518, .T. ) ;
#5299 = UNCERTAINTY_MEASURE_WITH_UNIT (LENGTH_MEASURE( 1.000000000000000082E-05 ), #13099, 'distance_accuracy_value', 'NONE');
#5300 = VERTEX_POINT ( 'NONE', #7093 ) ;
#5301 = DIRECTION ( 'NONE',  ( 1.000000000000000000, 1.746418240983389920E-16, 1.110223024625159992E-16 ) ) ;
#5302 = VECTOR ( 'NONE', #17915, 1000.000000000000000 ) ;
#5303 = CARTESIAN_POINT ( 'NONE',  ( -1.428515267734880023, -5.268855932203390324, 2.829745655876930055 ) ) ;
#5304 = LINE ( 'NONE', #951, #14705 ) ;
#5305 = PLANE ( 'NONE',  #15882 ) ;
#5306 = LINE ( 'NONE', #13643, #15289 ) ;
#5307 = CARTESIAN_POINT ( 'NONE',  ( 1.777964140657680048, -0.8689925102520590361, 6.241943319976220650 ) ) ;
#5308 = ADVANCED_FACE ( 'NONE', ( #12734 ), #9947, .F. ) ;
#5309 = LINE ( 'NONE', #17778, #5238 ) ;
#5310 = CARTESIAN_POINT ( 'NONE',  ( -2.051973656473811136, -4.917313796054240349, 4.634380218157504672 ) ) ;
#5311 = CARTESIAN_POINT ( 'NONE',  ( 1.851073041990159984, -0.1067796610169499949, 6.153284478378259870 ) ) ;
#5312 = EDGE_CURVE ( 'NONE', #4421, #2415, #16976, .T. ) ;
#5313 = CARTESIAN_POINT ( 'NONE',  ( 2.340070819011249803, -0.3800847457627120063, 4.950151441910540129 ) ) ;
#5314 = VECTOR ( 'NONE', #15118, 1000.000000000000000 ) ;
#5315 = ORIENTED_EDGE ( 'NONE', *, *, #14128, .T. ) ;
#5316 = EDGE_CURVE ( 'NONE', #1663, #4341, #4822, .T. ) ;
#5317 = CARTESIAN_POINT ( 'NONE',  ( -1.932035991685910004, -0.2610169491525428653, 2.884370051397200818 ) ) ;
#5318 = EDGE_LOOP ( 'NONE', ( #4859, #14469, #3158, #1165 ) ) ;
#5319 = ADVANCED_FACE ( 'NONE', ( #584, #10203 ), #6306, .F. ) ;
#5320 = LINE ( 'NONE', #10966, #17668 ) ;
#5321 = CARTESIAN_POINT ( 'NONE',  ( -0.8189529353761558772, -1.777235753495300052, 2.493631540942750302 ) ) ;
#5322 =( NAMED_UNIT ( * ) PLANE_ANGLE_UNIT ( ) SI_UNIT ( $, .RADIAN. ) );
#5323 = CARTESIAN_POINT ( 'NONE',  ( 2.351526912647309953, -5.373093220338979847, 4.606040641882800379 ) ) ;
#5324 = CARTESIAN_POINT ( 'NONE',  ( -2.550815101416269659, -1.404623140882690580, 5.432431574543720387 ) ) ;
#5325 = ORIENTED_EDGE ( 'NONE', *, *, #8622, .F. ) ;
#5326 = CARTESIAN_POINT ( 'NONE',  ( -1.670747221194380128, -5.103620102360550526, 3.047345349617600174 ) ) ;
#5327 = AXIS2_PLACEMENT_3D ( 'NONE', #6007, #1761, #545 ) ;
#5328 = CARTESIAN_POINT ( 'NONE',  ( 1.381042549632460092, -4.059488005747549977, 6.605640880016110827 ) ) ;
#5329 = CARTESIAN_POINT ( 'NONE',  ( -0.04351999560413650353, -4.521412895153344103, 7.353529668759054339 ) ) ;
#5330 = DIRECTION ( 'NONE',  ( 1.000000000000000000, 0.000000000000000000, -7.401486830834370362E-16 ) ) ;
#5331 = DIRECTION ( 'NONE',  ( 3.700743415417190112E-16, -1.000000000000000000, 8.217301096052200103E-32 ) ) ;
#5332 = DIRECTION ( 'NONE',  ( 0.000000000000000000, 0.000000000000000000, -1.000000000000000000 ) ) ;
#5333 = CARTESIAN_POINT ( 'NONE',  ( 1.138568046961060176, -1.237764246504700072, 6.408380708468512488 ) ) ;
#5334 = ADVANCED_BREP_SHAPE_REPRESENTATION ( '', ( #1876, #17681 ), #7087 ) ;
#5335 = CARTESIAN_POINT ( 'NONE',  ( 0.9499999999999999556, 2.299999999999999822, 7.599999999999999645 ) ) ;
#5336 = EDGE_LOOP ( 'NONE', ( #10609, #14089, #7080, #13092 ) ) ;
#5337 = DIRECTION ( 'NONE',  ( 0.000000000000000000, 0.000000000000000000, 1.000000000000000000 ) ) ;
#5338 = LINE ( 'NONE', #10984, #2322 ) ;
#5339 = CARTESIAN_POINT ( 'NONE',  ( 1.088937603231269646, -0.3266949152542383272, 2.959627624143540192 ) ) ;
#5340 = ADVANCED_FACE ( 'NONE', ( #17503 ), #8915, .T. ) ;
#5341 = CARTESIAN_POINT ( 'NONE',  ( -1.315254646989760134, -2.778632149891700376, 7.005042061779727547 ) ) ;
#5342 = LINE ( 'NONE', #3934, #5927 ) ;
#5343 = CARTESIAN_POINT ( 'NONE',  ( 2.030998484741458832, -5.381991525423726053, 4.999543428097175557 ) ) ;
#5344 = ORIENTED_EDGE ( 'NONE', *, *, #10953, .T. ) ;
#5345 = CARTESIAN_POINT ( 'NONE',  ( 1.889999999999999902, 3.500000000000000000, 0.5999999999999999778 ) ) ;
#5346 = CARTESIAN_POINT ( 'NONE',  ( 2.043308330018790198, -5.399788135593220240, 5.867646457774659652 ) ) ;
#5347 = CARTESIAN_POINT ( 'NONE',  ( -1.000000000000000000, -5.000000000000000000, 3.299999999999999822 ) ) ;
#5348 = ORIENTED_EDGE ( 'NONE', *, *, #7667, .T. ) ;
#5349 = CARTESIAN_POINT ( 'NONE',  ( 1.477796163681079911, -5.417584745762709986, 6.531563725478140015 ) ) ;
#5350 = CARTESIAN_POINT ( 'NONE',  ( 1.820241257191439921, -0.5196681859277348936, 3.208199930689769719 ) ) ;
#5351 = CARTESIAN_POINT ( 'NONE',  ( 1.576846334488021473, -3.892629111369556139, 2.565364356520400513 ) ) ;
#5352 = EDGE_CURVE ( 'NONE', #5832, #16609, #4650, .T. ) ;
#5353 = CARTESIAN_POINT ( 'NONE',  ( 1.438959988998139914E-16, 0.000000000000000000, 2.350000000000000089 ) ) ;
#5354 = VECTOR ( 'NONE', #14677, 1000.000000000000000 ) ;
#5355 = CARTESIAN_POINT ( 'NONE',  ( 0.03076623656506880661, -1.078587104846650213, 6.752792069673816400 ) ) ;
#5356 = CARTESIAN_POINT ( 'NONE',  ( 1.699999999999999956, 9.299999999999998934, 7.700000000000000178 ) ) ;
#5357 = DIRECTION ( 'NONE',  ( 6.162975822039159109E-32, 1.000000000000000000, 1.110223024625159992E-16 ) ) ;
#5358 = ORIENTED_EDGE ( 'NONE', *, *, #7772, .T. ) ;
#5359 = EDGE_CURVE ( 'NONE', #7455, #7321, #7616, .T. ) ;
#5360 = CARTESIAN_POINT ( 'NONE',  ( -0.7999999999998790301, 11.40000000000000036, -9.797174393178840942E-17 ) ) ;
#5361 = CARTESIAN_POINT ( 'NONE',  ( 2.130266475405040882, -0.3444915254237289615, 3.117337770017949428 ) ) ;
#5362 = CARTESIAN_POINT ( 'NONE',  ( 2.322440385110930094, -2.518620102360550117, 4.319189883157390497 ) ) ;
#5363 = DIRECTION ( 'NONE',  ( 7.401486830834370362E-16, 0.000000000000000000, 1.000000000000000000 ) ) ;
#5364 = CARTESIAN_POINT ( 'NONE',  ( -0.8147348917079838548, -0.2831443699174389095, 2.488757019513870627 ) ) ;
#5365 = CARTESIAN_POINT ( 'NONE',  ( -0.6640878839024662028, -5.462076271186444565, 7.269405042592523181 ) ) ;
#5366 = ORIENTED_EDGE ( 'NONE', *, *, #8711, .F. ) ;
#5367 = PRODUCT ( 'Top Metal Cover Plate', 'Top Metal Cover Plate', '', ( #14834 ) ) ;
#5368 = ORIENTED_EDGE ( 'NONE', *, *, #16510, .T. ) ;
#5369 = CARTESIAN_POINT ( 'NONE',  ( -1.707817112497179712, -5.188771186440678918, 6.319218296629480314 ) ) ;
#5370 = FACE_OUTER_BOUND ( 'NONE', #372, .T. ) ;
#5371 = VECTOR ( 'NONE', #2793, 1000.000000000000000 ) ;
#5372 = DIRECTION ( 'NONE',  ( 1.000000000000000000, -1.850371707708589879E-16, 0.000000000000000000 ) ) ;
#5373 = EDGE_CURVE ( 'NONE', #7510, #5452, #8994, .T. ) ;
#5374 = VERTEX_POINT ( 'NONE', #11600 ) ;
#5375 = CARTESIAN_POINT ( 'NONE',  ( -0.8934014991059870958, -4.614566048306490309, 6.877287176483410924 ) ) ;
#5376 = CARTESIAN_POINT ( 'NONE',  ( 1.652654650382400003, -0.7952867690272209522, 3.029252778805620050 ) ) ;
#5377 = CARTESIAN_POINT ( 'NONE',  ( 1.340185291429730974, -5.033893599512585304, 3.140995886557053307 ) ) ;
#5378 = LINE ( 'NONE', #2593, #12491 ) ;
#5379 = CARTESIAN_POINT ( 'NONE',  ( -2.267872052190610166, -1.843259742000189938, 4.071110468860649867 ) ) ;
#5380 = LINE ( 'NONE', #16669, #6974 ) ;
#5381 = CARTESIAN_POINT ( 'NONE',  ( -0.2739924515130059968, -2.984385868126320673, 6.734657214162127481 ) ) ;
#5382 = DIRECTION ( 'NONE',  ( -1.000000000000000000, 0.000000000000000000, -2.843808977011158816E-15 ) ) ;
#5383 = CARTESIAN_POINT ( 'NONE',  ( -1.372722144827311475, -0.2742238837839081067, 2.407683403867349803 ) ) ;
#5384 = ORIENTED_EDGE ( 'NONE', *, *, #12073, .F. ) ;
#5385 = PRESENTATION_STYLE_ASSIGNMENT (( #16589 ) ) ;
#5386 = ORIENTED_EDGE ( 'NONE', *, *, #682, .T. ) ;
#5387 = EDGE_LOOP ( 'NONE', ( #6407, #11713, #3997, #7827 ) ) ;
#5388 = ADVANCED_FACE ( 'NONE', ( #10389 ), #3350, .T. ) ;
#5389 = ORIENTED_EDGE ( 'NONE', *, *, #14580, .T. ) ;
#5390 = DIRECTION ( 'NONE',  ( 0.000000000000000000, 1.000000000000000000, 0.000000000000000000 ) ) ;
#5391 = CARTESIAN_POINT ( 'NONE',  ( 0.9707742057416334225, -5.126483050847465250, 6.508944043303927174 ) ) ;
#5392 = CARTESIAN_POINT ( 'NONE',  ( -1.576846334488060553, -1.707370888630439065, 2.565364356520430267 ) ) ;
#5393 = PLANE ( 'NONE',  #6988 ) ;
#5394 = DIRECTION ( 'NONE',  ( -3.392348130799090196E-16, 1.000000000000000000, 1.233581138472399909E-16 ) ) ;
#5395 = FACE_OUTER_BOUND ( 'NONE', #6299, .T. ) ;
#5396 = ADVANCED_FACE ( 'NONE', ( #8781 ), #4335, .T. ) ;
#5397 = CARTESIAN_POINT ( 'NONE',  ( 2.145694642186089851, -1.098034516774969882, 5.666819626392539888 ) ) ;
#5398 = CARTESIAN_POINT ( 'NONE',  ( 2.306642602145299925, -0.08453389830508530045, 5.166805192608480368 ) ) ;
#5399 = CARTESIAN_POINT ( 'NONE',  ( 1.194742379459969861, -0.4245762711864409789, 6.727584234649759409 ) ) ;
#5400 = EDGE_LOOP ( 'NONE', ( #13901, #14949, #15505, #7838 ) ) ;
#5401 = CARTESIAN_POINT ( 'NONE',  ( -2.650076489488250697, -0.2224576271186441134, 4.841243018609314497 ) ) ;
#5402 = LINE ( 'NONE', #9653, #11307 ) ;
#5403 = ORIENTED_EDGE ( 'NONE', *, *, #9175, .F. ) ;
#5404 = DIRECTION ( 'NONE',  ( 1.306144734853129823E-16, -1.000000000000000000, -1.306144734853129823E-16 ) ) ;
#5405 = CARTESIAN_POINT ( 'NONE',  ( -0.1226612266410539165, -2.662190708450249410, 7.050255286338656724 ) ) ;
#5406 = DIRECTION ( 'NONE',  ( 0.000000000000000000, 0.000000000000000000, 1.000000000000000000 ) ) ;
#5407 = CARTESIAN_POINT ( 'NONE',  ( 2.651721837666119796, -5.373093220338980736, 4.594045830208265180 ) ) ;
#5408 = CARTESIAN_POINT ( 'NONE',  ( 0.7756407636289058827, -1.008722239981790558, 7.238010066725317770 ) ) ;
#5409 = VERTEX_POINT ( 'NONE', #18202 ) ;
#5410 = EDGE_CURVE ( 'NONE', #2252, #2787, #12061, .T. ) ;
#5411 = CARTESIAN_POINT ( 'NONE',  ( 1.803891155489780074, -0.8185750573155089471, 3.188470185434109982 ) ) ;
#5412 = AXIS2_PLACEMENT_3D ( 'NONE', #9008, #14660, #4845 ) ;
#5413 = CARTESIAN_POINT ( 'NONE',  ( 1.981271652668330052, -3.966334852594400662, 5.970160748022399488 ) ) ;
#5414 = EDGE_CURVE ( 'NONE', #13613, #12574, #13045, .T. ) ;
#5415 = EDGE_CURVE ( 'NONE', #3830, #6319, #14525, .T. ) ;
#5416 = LINE ( 'NONE', #16892, #1372 ) ;
#5417 = DIRECTION ( 'NONE',  ( 0.000000000000000000, -0.4472135954999631458, 0.8944271909999133019 ) ) ;
#5418 = CARTESIAN_POINT ( 'NONE',  ( 1.699999999999999956, 9.299999999999998934, 7.599999999999999645 ) ) ;
#5419 = EDGE_CURVE ( 'NONE', #5295, #8002, #16792, .T. ) ;
#5420 = CARTESIAN_POINT ( 'NONE',  ( -1.616473591439278712, -1.610376859117309767, 5.965667796385567101 ) ) ;
#5421 = EDGE_CURVE ( 'NONE', #7849, #8434, #7759, .T. ) ;
#5422 = LINE ( 'NONE', #12736, #12348 ) ;
#5423 = ORIENTED_EDGE ( 'NONE', *, *, #16756, .F. ) ;
#5424 = DIRECTION ( 'NONE',  ( 0.000000000000000000, 4.485749594445070317E-16, 1.000000000000000000 ) ) ;
#5425 = DIRECTION ( 'NONE',  ( 1.000000000000000000, 1.708035422500239940E-16, 2.736911063134409557E-48 ) ) ;
#5426 = CARTESIAN_POINT ( 'NONE',  ( -0.4339619423229766348, -0.1601694915254239793, 6.706578715862737461 ) ) ;
#5427 = CARTESIAN_POINT ( 'NONE',  ( 1.071153154657499718, -2.545749267008810435, 7.128115444592616257 ) ) ;
#5428 = CARTESIAN_POINT ( 'NONE',  ( -0.5500000000000000444, 2.050000000000000266, 3.600000000000000089 ) ) ;
#5429 = CARTESIAN_POINT ( 'NONE',  ( -0.9345217207511814506, -5.211074464177369414, 2.212378604467589494 ) ) ;
#5430 = CARTESIAN_POINT ( 'NONE',  ( 0.9707742057416334225, -5.426483050847465073, 6.508944043303927174 ) ) ;
#5431 = EDGE_LOOP ( 'NONE', ( #8535, #1724, #1322, #8680 ) ) ;
#5432 = CARTESIAN_POINT ( 'NONE',  ( 2.116444151961469178, -0.05338983050847489337, 3.670839500609350381 ) ) ;
#5433 = FACE_OUTER_BOUND ( 'NONE', #5906, .T. ) ;
#5434 = DIRECTION ( 'NONE',  ( 0.000000000000000000, -0.4472135954999567065, -0.8944271909999164105 ) ) ;
#5435 = VERTEX_POINT ( 'NONE', #12018 ) ;
#5436 = CARTESIAN_POINT ( 'NONE',  ( -2.270487904532170198, -5.537711864406779760, 4.080813552109679776 ) ) ;
#5437 = CARTESIAN_POINT ( 'NONE',  ( -1.468674196027810686, -4.362235753495300905, 6.910454658870877509 ) ) ;
#5438 = CARTESIAN_POINT ( 'NONE',  ( -0.5385843327681574255, -3.683034516774964295, 2.101338688959530465 ) ) ;
#5439 = ADVANCED_FACE ( 'NONE', ( #9954 ), #6457, .F. ) ;
#5440 = DIRECTION ( 'NONE',  ( 6.083413833562510128E-16, -1.647588903766454767E-16, 1.000000000000000000 ) ) ;
#5441 = CARTESIAN_POINT ( 'NONE',  ( 2.004091155098369104, -0.6361096273691766445, 4.254443623407341057 ) ) ;
#5442 = LINE ( 'NONE', #7118, #8195 ) ;
#5443 = ORIENTED_EDGE ( 'NONE', *, *, #15088, .F. ) ;
#5444 = CARTESIAN_POINT ( 'NONE',  ( 1.764243121571529960, -5.142630151795009930, 2.935756878428469996 ) ) ;
#5445 = AXIS2_PLACEMENT_3D ( 'NONE', #3322, #8966, #2019 ) ;
#5446 = CARTESIAN_POINT ( 'NONE',  ( 1.000896394980339998, -0.4290254237288140260, 6.829956240957369751 ) ) ;
#5447 = CARTESIAN_POINT ( 'NONE',  ( 0.9719602541832789155, -2.844656138396589817, 6.843370931913530519 ) ) ;
#5448 = DIRECTION ( 'NONE',  ( 0.000000000000000000, 0.000000000000000000, 1.000000000000000000 ) ) ;
#5449 = CARTESIAN_POINT ( 'NONE',  ( -1.399999999999999911, -6.000000000000000000, 5.100000000000000533 ) ) ;
#5450 = CARTESIAN_POINT ( 'NONE',  ( -2.484260633728970546, -5.542161016949150643, 3.766563288620799366 ) ) ;
#5451 = ORIENTED_EDGE ( 'NONE', *, *, #15168, .F. ) ;
#5452 = VERTEX_POINT ( 'NONE', #17585 ) ;
#5453 = CARTESIAN_POINT ( 'NONE',  ( -1.149999999999999911, 9.299999999999998934, 7.599999999999999645 ) ) ;
#5454 = CARTESIAN_POINT ( 'NONE',  ( -0.3750000000000000000, 6.450000000000000178, 2.100000000000000089 ) ) ;
#5455 = CARTESIAN_POINT ( 'NONE',  ( -2.500000000000000000, 0.4000000000000000222, 7.649999999999999467 ) ) ;
#5456 = VERTEX_POINT ( 'NONE', #8003 ) ;
#5457 = CARTESIAN_POINT ( 'NONE',  ( 1.214457691475989920, -3.869340823081270031, 2.684103622926340194 ) ) ;
#5458 = EDGE_CURVE ( 'NONE', #14617, #12922, #11887, .T. ) ;
#5459 = CARTESIAN_POINT ( 'NONE',  ( 1.149999999999999911, 9.299999999999998934, 7.700000000000000178 ) ) ;
#5460 = CARTESIAN_POINT ( 'NONE',  ( 1.536215498768950027, -5.033893599512579975, 2.912754292501710474 ) ) ;
#5461 = VECTOR ( 'NONE', #18041, 1000.000000000000000 ) ;
#5462 = DIRECTION ( 'NONE',  ( -1.000000000000000000, 0.000000000000000000, 7.401486830834370362E-16 ) ) ;
#5463 = DIRECTION ( 'NONE',  ( 0.000000000000000000, 0.000000000000000000, 1.000000000000000000 ) ) ;
#5464 = CARTESIAN_POINT ( 'NONE',  ( -2.326448859701059746, -3.380286769027220029, 4.344498395672320434 ) ) ;
#5465 = CARTESIAN_POINT ( 'NONE',  ( 1.000000000000000000, 5.799999999999999822, 7.700000000000000178 ) ) ;
#5466 = CARTESIAN_POINT ( 'NONE',  ( -0.4194839839382230595, -3.683034516774964295, 2.690289814463939777 ) ) ;
#5467 = CARTESIAN_POINT ( 'NONE',  ( -1.899999999999999911, 0.5999999999999999778, 7.700000000000000178 ) ) ;
#5468 = CARTESIAN_POINT ( 'NONE',  ( 1.399999999999999911, 5.799999999999999822, 7.700000000000000178 ) ) ;
#5469 = EDGE_LOOP ( 'NONE', ( #7657, #8304, #15068, #310 ) ) ;
#5470 = CARTESIAN_POINT ( 'NONE',  ( 1.000000000000000000, 6.400000000000000355, 8.300000000000000711 ) ) ;
#5471 = ORIENTED_EDGE ( 'NONE', *, *, #4500, .F. ) ;
#5472 = ORIENTED_EDGE ( 'NONE', *, *, #4872, .T. ) ;
#5473 = PRODUCT_DEFINITION_CONTEXT ( 'detailed design', #4249, 'design' ) ;
#5474 = VERTEX_POINT ( 'NONE', #7621 ) ;
#5475 = FACE_OUTER_BOUND ( 'NONE', #729, .T. ) ;
#5476 = CARTESIAN_POINT ( 'NONE',  ( -1.846259792136611066, -5.246610169491530584, 3.802221692020929744 ) ) ;
#5477 = CARTESIAN_POINT ( 'NONE',  ( -2.653886076156968699, -1.474488005747551567, 4.698454755023434792 ) ) ;
#5478 = CARTESIAN_POINT ( 'NONE',  ( -1.399999999999999911, -5.500000000000000000, 6.100000000000000533 ) ) ;
#5479 = DIRECTION ( 'NONE',  ( 6.123233995736806712E-17, 0.000000000000000000, 1.000000000000000000 ) ) ;
#5480 = FACE_OUTER_BOUND ( 'NONE', #13735, .T. ) ;
#5481 = CARTESIAN_POINT ( 'NONE',  ( 3.371799150351489833E-16, 2.299999999999999822, 7.599999999999999645 ) ) ;
#5482 = CARTESIAN_POINT ( 'NONE',  ( 2.500000000000000000, 10.00000000000000000, -1.110223024625159893E-15 ) ) ;
#5483 = CARTESIAN_POINT ( 'NONE',  ( 1.652654650382400003, -0.7952867690272209522, 3.029252778805620050 ) ) ;
#5484 = CARTESIAN_POINT ( 'NONE',  ( -2.508228811380011081, -0.2091101694915259990, 5.566973598334550744 ) ) ;
#5485 = DIRECTION ( 'NONE',  ( 4.440892098500630106E-16, 0.000000000000000000, -1.000000000000000000 ) ) ;
#5486 = ORIENTED_EDGE ( 'NONE', *, *, #12230, .T. ) ;
#5487 = CARTESIAN_POINT ( 'NONE',  ( 1.526871680339569659, -0.04004237288135625850, 3.327650196883443101 ) ) ;
#5488 = CARTESIAN_POINT ( 'NONE',  ( 2.329383452786330189, -1.028169651910100013, 5.035735636132829818 ) ) ;
#5489 = ORIENTED_EDGE ( 'NONE', *, *, #5518, .T. ) ;
#5490 = CARTESIAN_POINT ( 'NONE',  ( 0.1749999999999999889, 9.299999999999998934, 1.600000000000000089 ) ) ;
#5491 = CARTESIAN_POINT ( 'NONE',  ( -2.169623098572329489, -2.941650167909711122, 5.611855963201050734 ) ) ;
#5492 = CARTESIAN_POINT ( 'NONE',  ( 0.000000000000000000, 0.000000000000000000, 0.000000000000000000 ) ) ;
#5493 = CARTESIAN_POINT ( 'NONE',  ( -2.354888465609351389, -5.502118644067805597, 5.923664702843871588 ) ) ;
#5494 = VECTOR ( 'NONE', #3990, 1000.000000000000000 ) ;
#5495 = ORIENTED_EDGE ( 'NONE', *, *, #9585, .F. ) ;
#5496 = FACE_OUTER_BOUND ( 'NONE', #11935, .T. ) ;
#5497 = CARTESIAN_POINT ( 'NONE',  ( 2.022304719220918479, -0.3667372881355940861, 4.346496488058688712 ) ) ;
#5498 = ORIENTED_EDGE ( 'NONE', *, *, #4503, .F. ) ;
#5499 = CARTESIAN_POINT ( 'NONE',  ( -0.9000000000000000222, -10.00000000000000000, 3.799999999999999822 ) ) ;
#5500 = LINE ( 'NONE', #4112, #6790 ) ;
#5501 = CARTESIAN_POINT ( 'NONE',  ( -0.1352600594605981310, -1.400782264522720366, 6.748562071049556188 ) ) ;
#5502 = PRODUCT_DEFINITION_SHAPE ( 'NONE', 'NONE',  #18298 ) ;
#5503 = DIRECTION ( 'NONE',  ( 1.000000000000000000, 0.000000000000000000, -6.049014748177260544E-16 ) ) ;
#5504 = AXIS2_PLACEMENT_3D ( 'NONE', #1102, #18023, #18107 ) ;
#5505 = ORIENTED_EDGE ( 'NONE', *, *, #10953, .F. ) ;
#5506 = CARTESIAN_POINT ( 'NONE',  ( 0.6207106781186539912, 6.450000000000000178, 2.628553390593269423 ) ) ;
#5507 = DIRECTION ( 'NONE',  ( 1.224646799147350002E-16, -1.000000000000000000, -6.123233995736769734E-17 ) ) ;
#5508 = CARTESIAN_POINT ( 'NONE',  ( 2.046424002475610404, -0.3711864406779670222, 4.536201610417760044 ) ) ;
#5509 = VECTOR ( 'NONE', #9296, 1000.000000000000000 ) ;
#5510 = EDGE_CURVE ( 'NONE', #6595, #4345, #14683, .T. ) ;
#5511 = VECTOR ( 'NONE', #10066, 1000.000000000000000 ) ;
#5512 = CARTESIAN_POINT ( 'NONE',  ( -0.2683982510037440927, -3.407415933675483899, 2.059720455735791322 ) ) ;
#5513 = AXIS2_PLACEMENT_3D ( 'NONE', #15945, #3245, #8889 ) ;
#5514 = CARTESIAN_POINT ( 'NONE',  ( 1.782460458101500889, -5.399788135593215799, 5.718585207845976015 ) ) ;
#5515 = VERTEX_POINT ( 'NONE', #11231 ) ;
#5516 = ADVANCED_FACE ( 'NONE', ( #6789 ), #12437, .T. ) ;
#5517 = CARTESIAN_POINT ( 'NONE',  ( -1.661700935788390288, -0.2625000000000000111, 3.038299064211610112 ) ) ;
#5518 = EDGE_CURVE ( 'NONE', #11846, #9094, #2626, .T. ) ;
#5519 = DIRECTION ( 'NONE',  ( 4.485749594445070317E-16, 0.000000000000000000, 1.000000000000000000 ) ) ;
#5520 = DIRECTION ( 'NONE',  ( -1.000000000000000000, 1.224646799147341128E-16, 0.000000000000000000 ) ) ;
#5521 = EDGE_CURVE ( 'NONE', #6586, #17729, #11039, .T. ) ;
#5522 = ORIENTED_EDGE ( 'NONE', *, *, #11147, .T. ) ;
#5523 = LINE ( 'NONE', #10062, #3156 ) ;
#5524 = CARTESIAN_POINT ( 'NONE',  ( -2.035218756299248977, -4.781424942684484591, 2.996768277952679860 ) ) ;
#5525 = AXIS2_PLACEMENT_3D ( 'NONE', #6519, #5331, #10879 ) ;
#5526 = AXIS2_PLACEMENT_3D ( 'NONE', #12999, #1877, #230 ) ;
#5527 = CYLINDRICAL_SURFACE ( 'NONE', #13491, 0.4166666666666670737 ) ;
#5528 = CARTESIAN_POINT ( 'NONE',  ( 2.028464043723889887, -0.7292627805223297344, 5.016599851465070259 ) ) ;
#5529 = VECTOR ( 'NONE', #8203, 1000.000000000000000 ) ;
#5530 = DIRECTION ( 'NONE',  ( 0.000000000000000000, 0.000000000000000000, 1.000000000000000000 ) ) ;
#5531 = ORIENTED_EDGE ( 'NONE', *, *, #9721, .T. ) ;
#5532 = VECTOR ( 'NONE', #2051, 1000.000000000000000 ) ;
#5533 = CIRCLE ( 'NONE', #15883, 0.2500000000000002220 ) ;
#5534 = CARTESIAN_POINT ( 'NONE',  ( -2.500000000000000000, 3.500000000000000000, 0.6099999999999999867 ) ) ;
#5535 = CARTESIAN_POINT ( 'NONE',  ( 1.378221871957440170, -0.4201271186440679872, 6.607619368096269596 ) ) ;
#5536 = CARTESIAN_POINT ( 'NONE',  ( -2.349464193210359930, -3.356998480738930368, 4.563019372514619754 ) ) ;
#5537 = CARTESIAN_POINT ( 'NONE',  ( -1.889999999999999902, 7.900000000000000355, 2.126957699879220439E-15 ) ) ;
#5538 = DIRECTION ( 'NONE',  ( 0.000000000000000000, 0.000000000000000000, -1.000000000000000000 ) ) ;
#5539 = CARTESIAN_POINT ( 'NONE',  ( -2.130266475405059090, -5.555508474576275724, 3.117337770017961418 ) ) ;
#5540 = ORIENTED_EDGE ( 'NONE', *, *, #7049, .F. ) ;
#5541 = EDGE_CURVE ( 'NONE', #16962, #410, #7076, .T. ) ;
#5542 = AXIS2_PLACEMENT_3D ( 'NONE', #4061, #9903, #12687 ) ;
#5543 = AXIS2_PLACEMENT_3D ( 'NONE', #10739, #10831, #16386 ) ;
#5544 = EDGE_LOOP ( 'NONE', ( #3326, #924, #17544, #10702 ) ) ;
#5545 = CARTESIAN_POINT ( 'NONE',  ( -2.270487904532169754, -5.237711864406779050, 4.080813552109680664 ) ) ;
#5546 =( LENGTH_UNIT ( ) NAMED_UNIT ( * ) SI_UNIT ( .MILLI., .METRE. ) );
#5547 = CARTESIAN_POINT ( 'NONE',  ( -1.889999999999999902, 7.299999999999999822, 1.321762070856419966E-15 ) ) ;
#5548 = AXIS2_PLACEMENT_3D ( 'NONE', #1392, #6276, #4884 ) ;
#5549 = ORIENTED_EDGE ( 'NONE', *, *, #7534, .T. ) ;
#5550 = CIRCLE ( 'NONE', #7035, 0.1000000000000003247 ) ;
#5551 = VECTOR ( 'NONE', #6303, 1000.000000000000000 ) ;
#5552 = CARTESIAN_POINT ( 'NONE',  ( 1.401708661791409849, -4.358394877135329359, 6.590491606684049763 ) ) ;
#5553 = CARTESIAN_POINT ( 'NONE',  ( -0.009452110982655099330, -5.299807955295455564, 2.649999999999998579 ) ) ;
#5554 = CARTESIAN_POINT ( 'NONE',  ( -0.8740908734716290596, 4.154758922476410099, 8.300000000000000711 ) ) ;
#5555 = CARTESIAN_POINT ( 'NONE',  ( 1.889999999999999902, 4.700000000000000178, 0.6099999999999999867 ) ) ;
#5556 = VECTOR ( 'NONE', #5656, 1000.000000000000000 ) ;
#5557 = CARTESIAN_POINT ( 'NONE',  ( -0.6918414964982418924, -3.659746228486680408, 2.450533167346770291 ) ) ;
#5558 = VECTOR ( 'NONE', #18007, 1000.000000000000000 ) ;
#5559 = DIRECTION ( 'NONE',  ( -0.000000000000000000, 1.000000000000000000, 0.000000000000000000 ) ) ;
#5560 = CARTESIAN_POINT ( 'NONE',  ( 1.736825397686149852, -3.985782264522713447, 3.605313112995111702 ) ) ;
#5561 = FACE_BOUND ( 'NONE', #18066, .T. ) ;
#5562 = COLOUR_RGB ( '', 0.08235294, 0.09019608, 0.10196078) ;
#5563 = ORIENTED_EDGE ( 'NONE', *, *, #86, .T. ) ;
#5564 = LINE ( 'NONE', #12868, #2365 ) ;
#5565 = ORIENTED_EDGE ( 'NONE', *, *, #7447, .T. ) ;
#5566 = AXIS2_PLACEMENT_3D ( 'NONE', #4068, #13627, #15392 ) ;
#5567 = EDGE_CURVE ( 'NONE', #7602, #7108, #12717, .T. ) ;
#5568 = EDGE_LOOP ( 'NONE', ( #901, #9935, #11326, #7967 ) ) ;
#5569 = VERTEX_POINT ( 'NONE', #5853 ) ;
#5570 = AXIS2_PLACEMENT_3D ( 'NONE', #15438, #18159, #6814 ) ;
#5571 = ORIENTED_EDGE ( 'NONE', *, *, #11390, .F. ) ;
#5572 = CARTESIAN_POINT ( 'NONE',  ( 0.5500000000000000444, -2.399999999999999911, 3.299999999999999822 ) ) ;
#5573 = CIRCLE ( 'NONE', #15045, 0.6100000000000000977 ) ;
#5574 = CARTESIAN_POINT ( 'NONE',  ( -1.392553072310521278, -5.264406779661021218, 3.191531554476531252 ) ) ;
#5575 = CARTESIAN_POINT ( 'NONE',  ( -1.370891210199559618, -1.730659176918718956, 2.427606771969371469 ) ) ;
#5576 = PLANE ( 'NONE',  #2898 ) ;
#5577 = CARTESIAN_POINT ( 'NONE',  ( -2.500000000000000000, 0.7500000000000000000, 7.649999999999999467 ) ) ;
#5578 = VECTOR ( 'NONE', #15644, 1000.000000000000000 ) ;
#5579 = CARTESIAN_POINT ( 'NONE',  ( -1.850000000000000089, -5.599999999999999645, 6.899999999999999467 ) ) ;
#5580 = CARTESIAN_POINT ( 'NONE',  ( 1.800000000000000044, 0.5999999999999999778, 7.599999999999999645 ) ) ;
#5581 = PLANE ( 'NONE',  #5255 ) ;
#5582 = CARTESIAN_POINT ( 'NONE',  ( 2.322440385110930094, -2.518620102360550117, 4.319189883157390497 ) ) ;
#5583 = CARTESIAN_POINT ( 'NONE',  ( -1.928470600873600782, -3.127956474216021299, 3.995796205495660391 ) ) ;
#5584 = CARTESIAN_POINT ( 'NONE',  ( -2.293398556041709835, -0.2358050847457629773, 4.171956209133480975 ) ) ;
#5585 = AXIS2_PLACEMENT_3D ( 'NONE', #11956, #14552, #14633 ) ;
#5586 = DIRECTION ( 'NONE',  ( -1.000000000000000000, -4.014365738757630620E-15, -1.254489293361759815E-16 ) ) ;
#5587 = CARTESIAN_POINT ( 'NONE',  ( -2.000624272291700034, -0.5358050847457624943, 4.239366054776020576 ) ) ;
#5588 = FACE_OUTER_BOUND ( 'NONE', #8739, .T. ) ;
#5589 = ORIENTED_EDGE ( 'NONE', *, *, #17058, .F. ) ;
#5590 = ADVANCED_FACE ( 'NONE', ( #7427 ), #119, .F. ) ;
#5591 = CARTESIAN_POINT ( 'NONE',  ( 0.2818998297622880012, -1.354205687946139935, 7.036509827384409554 ) ) ;
#5592 = ORIENTED_EDGE ( 'NONE', *, *, #11971, .T. ) ;
#5593 = VECTOR ( 'NONE', #15093, 1000.000000000000000 ) ;
#5594 = VECTOR ( 'NONE', #6045, 1000.000000000000000 ) ;
#5595 = ORIENTED_EDGE ( 'NONE', *, *, #13568, .T. ) ;
#5596 = CARTESIAN_POINT ( 'NONE',  ( 1.948278411993589421, -2.406019537279080467, 6.020210936495999476 ) ) ;
#5597 = CARTESIAN_POINT ( 'NONE',  ( 1.932035991685901122, -5.338983050847455836, 2.884370051397200818 ) ) ;
#5598 = ORIENTED_EDGE ( 'NONE', *, *, #16735, .T. ) ;
#5599 =( GEOMETRIC_REPRESENTATION_CONTEXT ( 3 ) GLOBAL_UNCERTAINTY_ASSIGNED_CONTEXT ( ( #13805 ) ) GLOBAL_UNIT_ASSIGNED_CONTEXT ( ( #6078, #15511, #2731 ) ) REPRESENTATION_CONTEXT ( 'NONE', 'WORKASPACE' ) );
#5600 = CARTESIAN_POINT ( 'NONE',  ( 1.480680413335799805, -1.214475958216410190, 6.529298007719799735 ) ) ;
#5601 = CARTESIAN_POINT ( 'NONE',  ( 1.821706171509118954, -0.3978813559322044724, 5.646608543709396244 ) ) ;
#5602 = EDGE_LOOP ( 'NONE', ( #11424, #948, #9260, #17946 ) ) ;
#5603 = PLANE ( 'NONE',  #6994 ) ;
#5604 = CARTESIAN_POINT ( 'NONE',  ( -0.5500000000000000444, 3.050000000000000266, 3.200000000000000178 ) ) ;
#5605 = AXIS2_PLACEMENT_3D ( 'NONE', #11673, #15851, #567 ) ;
#5606 = CARTESIAN_POINT ( 'NONE',  ( 1.996236309555640798, -1.051457940198389673, 5.179523137126535559 ) ) ;
#5607 = CARTESIAN_POINT ( 'NONE',  ( 1.399999999999999911, -9.500000000000000000, 3.299999999999999822 ) ) ;
#5608 = CARTESIAN_POINT ( 'NONE',  ( 2.354888465609351389, -0.3978813559322044724, 5.923664702843856489 ) ) ;
#5609 = VERTEX_POINT ( 'NONE', #10114 ) ;
#5610 = CARTESIAN_POINT ( 'NONE',  ( -2.616666666666669805, -4.318079751576579732E-16, 4.000000000000000000 ) ) ;
#5611 = CARTESIAN_POINT ( 'NONE',  ( 7.347880794884119736E-16, -6.000000000000000000, -3.673940397442060361E-16 ) ) ;
#5612 = CARTESIAN_POINT ( 'NONE',  ( -1.289141334274979789, -0.1824152542372889096, 6.297747079672432413 ) ) ;
#5613 = PLANE ( 'NONE',  #303 ) ;
#5614 = CARTESIAN_POINT ( 'NONE',  ( 0.1785884594055070773, -4.199217735477280833, 7.347870815423032553 ) ) ;
#5615 = ORIENTED_EDGE ( 'NONE', *, *, #5421, .F. ) ;
#5616 = CARTESIAN_POINT ( 'NONE',  ( -1.294880990849879732, -4.829629811528119987, 3.097365952343163364 ) ) ;
#5617 = CARTESIAN_POINT ( 'NONE',  ( -1.821706171509118954, -5.202118644067803999, 5.646608543709410455 ) ) ;
#5618 = ORIENTED_EDGE ( 'NONE', *, *, #6937, .T. ) ;
#5619 = CARTESIAN_POINT ( 'NONE',  ( 1.750316316486830059, -0.04004237288135629319, 3.126818518378580158 ) ) ;
#5620 = CARTESIAN_POINT ( 'NONE',  ( 2.155845792290829621, -5.355296610169490101, 3.756158857535770057 ) ) ;
#5621 = AXIS2_PLACEMENT_3D ( 'NONE', #8499, #12484, #1281 ) ;
#5622 = CARTESIAN_POINT ( 'NONE',  ( -1.889999999999999902, 7.299999999999999822, 0.6099999999999999867 ) ) ;
#5623 = ORIENTED_EDGE ( 'NONE', *, *, #4045, .F. ) ;
#5624 = DIRECTION ( 'NONE',  ( 6.123233995736767268E-17, -1.000000000000000000, 0.000000000000000000 ) ) ;
#5625 = CARTESIAN_POINT ( 'NONE',  ( 1.282210379528780031, -0.9388573751169240200, 6.673494927815259992 ) ) ;
#5626 = LINE ( 'NONE', #11269, #13827 ) ;
#5627 = CARTESIAN_POINT ( 'NONE',  ( -1.971820545011380821, -1.544352870612421880, 4.128313389260230615 ) ) ;
#5628 = EDGE_CURVE ( 'NONE', #5515, #6950, #15897, .T. ) ;
#5629 = ORIENTED_EDGE ( 'NONE', *, *, #4986, .F. ) ;
#5630 = EDGE_CURVE ( 'NONE', #9279, #17265, #302, .T. ) ;
#5631 = AXIS2_PLACEMENT_3D ( 'NONE', #10153, #17091, #613 ) ;
#5632 = DIRECTION ( 'NONE',  ( 1.850371707708589879E-16, 0.000000000000000000, -1.000000000000000000 ) ) ;
#5633 = CARTESIAN_POINT ( 'NONE',  ( -0.7093417302541390468, -0.4646186440677970153, 6.943956659919700236 ) ) ;
#5634 = CARTESIAN_POINT ( 'NONE',  ( -0.8986180677147959095, -3.636457940198390304, 2.524860635301629852 ) ) ;
#5635 = DIRECTION ( 'NONE',  ( 0.000000000000000000, 0.000000000000000000, 1.000000000000000000 ) ) ;
#5636 = LINE ( 'NONE', #15648, #16273 ) ;
#5637 = CARTESIAN_POINT ( 'NONE',  ( -0.4221287159901280228, -5.457627118644064801, 7.320050063945812369 ) ) ;
#5638 = ORIENTED_EDGE ( 'NONE', *, *, #6822, .F. ) ;
#5639 = ORIENTED_EDGE ( 'NONE', *, *, #5918, .T. ) ;
#5640 = CARTESIAN_POINT ( 'NONE',  ( -2.345900685764729765, -5.228813559322029292, 4.512231114381338948 ) ) ;
#5641 = CARTESIAN_POINT ( 'NONE',  ( -1.800000000000000044, 0.5999999999999999778, 7.599999999999999645 ) ) ;
#5642 = ORIENTED_EDGE ( 'NONE', *, *, #18149, .F. ) ;
#5643 = VECTOR ( 'NONE', #10989, 1000.000000000000000 ) ;
#5644 = CARTESIAN_POINT ( 'NONE',  ( -0.1785884594054470975, -1.400782264522720366, 7.347870815423047652 ) ) ;
#5645 = EDGE_CURVE ( 'NONE', #18075, #15355, #10284, .T. ) ;
#5646 = CARTESIAN_POINT ( 'NONE',  ( 0.2254033459420760055, -0.6247245358507570456, 2.348900562125120217 ) ) ;
#5647 = CARTESIAN_POINT ( 'NONE',  ( 1.534924416212170017, -5.333856471232000018, 2.911460733964629899 ) ) ;
#5648 = CARTESIAN_POINT ( 'NONE',  ( 7.233457020361919865E-16, 4.000000000000000000, 5.100000000000000533 ) ) ;
#5649 = CARTESIAN_POINT ( 'NONE',  ( -2.192143888961709752, -1.381334852594400031, 5.556300681753639559 ) ) ;
#5650 = EDGE_CURVE ( 'NONE', #10555, #7787, #6948, .T. ) ;
#5651 = CARTESIAN_POINT ( 'NONE',  ( 1.889999999999999902, 8.500000000000000000, 1.696109213374460111E-16 ) ) ;
#5652 = CARTESIAN_POINT ( 'NONE',  ( 2.192143888961729736, -4.218665147405599392, 5.556300681753580051 ) ) ;
#5653 = EDGE_CURVE ( 'NONE', #4106, #13454, #1860, .T. ) ;
#5654 = DIRECTION ( 'NONE',  ( -1.000000000000000000, -1.776356839400250070E-15, 0.000000000000000000 ) ) ;
#5655 = CARTESIAN_POINT ( 'NONE',  ( -0.6470883152343470668, -3.030962444702889780, 6.648378442427256729 ) ) ;
#5656 = DIRECTION ( 'NONE',  ( -1.000000000000000000, 0.000000000000000000, 0.000000000000000000 ) ) ;
#5657 = DIRECTION ( 'NONE',  ( 0.000000000000000000, 0.000000000000000000, 1.000000000000000000 ) ) ;
#5658 = AXIS2_PLACEMENT_3D ( 'NONE', #11830, #8769, #13125 ) ;
#5659 = ORIENTED_EDGE ( 'NONE', *, *, #6875, .F. ) ;
#5660 = CARTESIAN_POINT ( 'NONE',  ( 0.009452039534068971960, -5.000193177104105047, 2.350000000173209536 ) ) ;
#5661 = ORIENTED_EDGE ( 'NONE', *, *, #10723, .F. ) ;
#5662 = FACE_OUTER_BOUND ( 'NONE', #15465, .T. ) ;
#5663 = CARTESIAN_POINT ( 'NONE',  ( -1.850000000000000089, -5.599999999999999645, 6.400000000000000355 ) ) ;
#5664 = ORIENTED_EDGE ( 'NONE', *, *, #4590, .F. ) ;
#5665 = DIRECTION ( 'NONE',  ( 0.000000000000000000, 0.000000000000000000, 1.000000000000000000 ) ) ;
#5666 = CARTESIAN_POINT ( 'NONE',  ( -0.4000000000000000222, -1.399999999999999911, 6.100000000000000533 ) ) ;
#5667 = ORIENTED_EDGE ( 'NONE', *, *, #3511, .F. ) ;
#5668 = CARTESIAN_POINT ( 'NONE',  ( 1.449568901432419343, -5.037500000000000533, 3.250431098567584165 ) ) ;
#5669 = CARTESIAN_POINT ( 'NONE',  ( 1.837442528958791010, -2.056695212954759100, 2.785079989718789673 ) ) ;
#5670 = DIRECTION ( 'NONE',  ( -0.7071067811865489050, 0.000000000000000000, 0.7071067811865461294 ) ) ;
#5671 = CARTESIAN_POINT ( 'NONE',  ( 0.9499999999999999556, 2.299999999999999822, 7.599999999999999645 ) ) ;
#5672 = CARTESIAN_POINT ( 'NONE',  ( -2.616666666666669805, -4.318079751576579732E-16, 4.000000000000000000 ) ) ;
#5673 = LINE ( 'NONE', #5580, #6670 ) ;
#5674 = ADVANCED_FACE ( 'NONE', ( #14196 ), #11580, .T. ) ;
#5675 = DIRECTION ( 'NONE',  ( 1.224646799147351975E-16, -1.000000000000000000, -6.123233995736789455E-17 ) ) ;
#5676 = CARTESIAN_POINT ( 'NONE',  ( 0.6673090596498160165, -2.239160642901090181, 2.443133963569570355 ) ) ;
#5677 = CARTESIAN_POINT ( 'NONE',  ( 0.4625564304288019568, -2.592325843585391532, 6.700235833919842676 ) ) ;
#5678 = CARTESIAN_POINT ( 'NONE',  ( 1.614765845140360589, -0.1067796610169500227, 5.967758800287426446 ) ) ;
#5679 = DIRECTION ( 'NONE',  ( 7.656710514656250048E-17, -0.9659258262890690894, -0.2588190451025180749 ) ) ;
#5680 = PLANE ( 'NONE',  #13280 ) ;
#5681 = EDGE_LOOP ( 'NONE', ( #17526, #11833, #11028, #12614 ) ) ;
#5682 = CARTESIAN_POINT ( 'NONE',  ( -1.943632316591239917, -0.2536016949152539723, 3.373048379518170048 ) ) ;
#5683 = CARTESIAN_POINT ( 'NONE',  ( -0.3159454637156809409, -2.984385868126319785, 7.032150113402090064 ) ) ;
#5684 = VERTEX_POINT ( 'NONE', #17212 ) ;
#5685 = VERTEX_POINT ( 'NONE', #13153 ) ;
#5686 = EDGE_CURVE ( 'NONE', #4743, #14568, #8636, .T. ) ;
#5687 = CARTESIAN_POINT ( 'NONE',  ( -1.991984774470508590, -1.614217735477280202, 3.446707398186050764 ) ) ;
#5688 = DIRECTION ( 'NONE',  ( 0.000000000000000000, 0.000000000000000000, 1.000000000000000000 ) ) ;
#5689 = CARTESIAN_POINT ( 'NONE',  ( 2.043014502273419186, -5.341949152542365908, 3.006203457898239062 ) ) ;
#5690 = ORIENTED_EDGE ( 'NONE', *, *, #5645, .F. ) ;
#5691 = CARTESIAN_POINT ( 'NONE',  ( 0.06276132972186961034, -1.377493976234430040, 7.052616990284530374 ) ) ;
#5692 = EDGE_CURVE ( 'NONE', #16402, #12675, #12806, .T. ) ;
#5693 = CARTESIAN_POINT ( 'NONE',  ( 1.889104232906359870, -0.3444915254237289615, 3.296507079072520163 ) ) ;
#5694 = ORIENTED_EDGE ( 'NONE', *, *, #14236, .F. ) ;
#5695 = CIRCLE ( 'NONE', #7180, 0.2500000000000002220 ) ;
#5696 = EDGE_CURVE ( 'NONE', #5685, #4195, #11409, .T. ) ;
#5697 = CARTESIAN_POINT ( 'NONE',  ( 0.6500000000000000222, 6.450000000000000178, 2.699264068711930253 ) ) ;
#5698 = PLANE ( 'NONE',  #867 ) ;
#5699 = CARTESIAN_POINT ( 'NONE',  ( 1.404946080800569375, -2.355602084342530933, 3.202993536195909208 ) ) ;
#5700 = DIRECTION ( 'NONE',  ( -1.000000000000000000, 0.000000000000000000, 1.586032892321649771E-16 ) ) ;
#5701 = CARTESIAN_POINT ( 'NONE',  ( 1.973760952634081134, -0.3400423728813561364, 2.925986839873718992 ) ) ;
#5702 = ORIENTED_EDGE ( 'NONE', *, *, #10980, .F. ) ;
#5703 = CARTESIAN_POINT ( 'NONE',  ( 1.699999999999999956, 9.299999999999998934, 7.599999999999999645 ) ) ;
#5704 = CARTESIAN_POINT ( 'NONE',  ( -0.7982439214406890082, -0.4690677966101705065, 6.591424794228156081 ) ) ;
#5705 = ORIENTED_EDGE ( 'NONE', *, *, #5510, .F. ) ;
#5706 = CARTESIAN_POINT ( 'NONE',  ( -0.1458667720079689645, -4.981295943764795453, 2.649245313618650677 ) ) ;
#5707 = CARTESIAN_POINT ( 'NONE',  ( 2.058670345754650022, -5.350847457627120107, 3.559656372813920111 ) ) ;
#5708 = EDGE_LOOP ( 'NONE', ( #2495, #6723, #1540, #13155 ) ) ;
#5709 = DIRECTION ( 'NONE',  ( -1.644774851296529842E-16, 1.000000000000000000, 0.000000000000000000 ) ) ;
#5710 = DIRECTION ( 'NONE',  ( -1.110223024625160090E-15, -1.000000000000000000, 0.000000000000000000 ) ) ;
#5711 = CARTESIAN_POINT ( 'NONE',  ( -1.000000000000000000, 5.400000000000000355, 8.300000000000000711 ) ) ;
#5712 = VERTEX_POINT ( 'NONE', #10027 ) ;
#5713 = DIRECTION ( 'NONE',  ( 1.000000000000000000, 0.000000000000000000, 0.000000000000000000 ) ) ;
#5714 = CARTESIAN_POINT ( 'NONE',  ( 1.286937324407710026, -2.010118636378180224, 2.729584305145179801 ) ) ;
#5715 = CYLINDRICAL_SURFACE ( 'NONE', #5840, 0.4000000000000001887 ) ;
#5716 = CARTESIAN_POINT ( 'NONE',  ( 0.6050872056802326648, -1.940253771513320125, 2.738171435586128410 ) ) ;
#5717 = AXIS2_PLACEMENT_3D ( 'NONE', #17090, #17001, #15728 ) ;
#5718 = ORIENTED_EDGE ( 'NONE', *, *, #16364, .T. ) ;
#5719 = LINE ( 'NONE', #5360, #8539 ) ;
#5720 = CARTESIAN_POINT ( 'NONE',  ( 1.192209327851080136, -0.02224576271186471527, 2.329031440774910422 ) ) ;
#5721 = CARTESIAN_POINT ( 'NONE',  ( 0.6096110657044089276, -3.799475958216410376, 2.426869991387509806 ) ) ;
#5722 = FACE_OUTER_BOUND ( 'NONE', #4916, .T. ) ;
#5723 = DIRECTION ( 'NONE',  ( 0.000000000000000000, 0.000000000000000000, 1.000000000000000000 ) ) ;
#5724 = CARTESIAN_POINT ( 'NONE',  ( -2.560337424259679917, -5.237711864406785267, 4.001768473655595848 ) ) ;
#5725 = ORIENTED_EDGE ( 'NONE', *, *, #7772, .F. ) ;
#5726 = ORIENTED_EDGE ( 'NONE', *, *, #10487, .T. ) ;
#5727 = PLANE ( 'NONE',  #7424 ) ;
#5728 = CYLINDRICAL_SURFACE ( 'NONE', #16526, 0.7000000000000000666 ) ;
#5729 = DIRECTION ( 'NONE',  ( 0.000000000000000000, 0.000000000000000000, 1.000000000000000000 ) ) ;
#5730 = ORIENTED_EDGE ( 'NONE', *, *, #13350, .F. ) ;
#5731 = EDGE_CURVE ( 'NONE', #6864, #7679, #13833, .T. ) ;
#5732 = CARTESIAN_POINT ( 'NONE',  ( 2.629224451638851434, -0.9583047870452394701, 4.339039509243856507 ) ) ;
#5733 = SURFACE_STYLE_FILL_AREA ( #87 ) ;
#5734 = CARTESIAN_POINT ( 'NONE',  ( 0.5677251586959709551, -5.311531839079339790, 2.399563163165729929 ) ) ;
#5735 = PLANE ( 'NONE',  #9221 ) ;
#5736 = CARTESIAN_POINT ( 'NONE',  ( -1.869848057046539891, -1.311469987729539932, 6.129130480762059463 ) ) ;
#5737 = DIRECTION ( 'NONE',  ( -0.000000000000000000, 1.000000000000000000, 0.000000000000000000 ) ) ;
#5738 = CARTESIAN_POINT ( 'NONE',  ( -0.4735094604798580353, -4.567989471729919870, 7.005327412390699671 ) ) ;
#5739 = LINE ( 'NONE', #4159, #14373 ) ;
#5740 = CARTESIAN_POINT ( 'NONE',  ( 1.503314099254039471, -3.939205687946139900, 3.301805249039985402 ) ) ;
#5741 = DIRECTION ( 'NONE',  ( -2.220446049250309876E-16, 0.000000000000000000, 1.000000000000000000 ) ) ;
#5742 = CARTESIAN_POINT ( 'NONE',  ( 1.596341326794969984, -0.3355932203389830337, 2.970780074643809776 ) ) ;
#5743 = ORIENTED_EDGE ( 'NONE', *, *, #10841, .F. ) ;
#5744 = DIRECTION ( 'NONE',  ( 4.440892098500630106E-16, -1.000000000000000000, 0.000000000000000000 ) ) ;
#5745 = VERTEX_POINT ( 'NONE', #7248 ) ;
#5746 = EDGE_CURVE ( 'NONE', #9328, #14177, #12889, .T. ) ;
#5747 = CARTESIAN_POINT ( 'NONE',  ( 1.750000000000000000, 11.40000000000000036, 7.599999999999999645 ) ) ;
#5748 = EDGE_LOOP ( 'NONE', ( #101, #3135, #17789, #8554 ) ) ;
#5749 = LINE ( 'NONE', #7155, #17663 ) ;
#5750 = EDGE_CURVE ( 'NONE', #13435, #8906, #4456, .T. ) ;
#5751 = ORIENTED_EDGE ( 'NONE', *, *, #5731, .T. ) ;
#5752 = VECTOR ( 'NONE', #6274, 1000.000000000000000 ) ;
#5753 = EDGE_CURVE ( 'NONE', #8619, #9205, #6736, .T. ) ;
#5754 = CARTESIAN_POINT ( 'NONE',  ( 1.869504824896970119, -5.095338983050850423, 5.548311746956850143 ) ) ;
#5755 = EDGE_CURVE ( 'NONE', #4807, #17154, #10546, .T. ) ;
#5756 = CARTESIAN_POINT ( 'NONE',  ( 0.2750000000000004663, 2.299999999999999822, 7.599999999999999645 ) ) ;
#5757 = DIRECTION ( 'NONE',  ( 0.000000000000000000, 0.000000000000000000, -1.000000000000000000 ) ) ;
#5758 = LINE ( 'NONE', #2618, #8533 ) ;
#5759 = CARTESIAN_POINT ( 'NONE',  ( -1.882879255550339082, -5.103620102360555855, 2.835213315261639000 ) ) ;
#5760 = DIRECTION ( 'NONE',  ( 0.7071067811865466846, 0.000000000000000000, -0.7071067811865483499 ) ) ;
#5761 = DIRECTION ( 'NONE',  ( 1.000000000000000000, 0.000000000000000000, 0.000000000000000000 ) ) ;
#5762 = CARTESIAN_POINT ( 'NONE',  ( 2.301223891756920104, -2.611773255513699876, 5.193066210047949660 ) ) ;
#5763 = CARTESIAN_POINT ( 'NONE',  ( -0.8493734496527890476, -2.755343861603408939, 6.569081749323187225 ) ) ;
#5764 = CARTESIAN_POINT ( 'NONE',  ( 1.202278654260740876, -0.1201271186440679706, 6.364093491318035589 ) ) ;
#5765 = DIRECTION ( 'NONE',  ( 0.000000000000000000, 0.000000000000000000, 1.000000000000000000 ) ) ;
#5766 = CARTESIAN_POINT ( 'NONE',  ( -1.880631435828179265, -0.5447033898305090327, 3.876649216148230437 ) ) ;
#5767 = CARTESIAN_POINT ( 'NONE',  ( -1.399999999999999911, -6.000000000000000000, 3.299999999999999822 ) ) ;
#5768 = ORIENTED_EDGE ( 'NONE', *, *, #4038, .T. ) ;
#5769 = EDGE_CURVE ( 'NONE', #16414, #17164, #6112, .T. ) ;
#5770 = CARTESIAN_POINT ( 'NONE',  ( 0.5664586606772286093, -0.01334745762711899916, 2.726727161522279452 ) ) ;
#5771 = CARTESIAN_POINT ( 'NONE',  ( -2.345213174852959881, -1.796683165423619943, 4.503223853122380049 ) ) ;
#5772 = EDGE_LOOP ( 'NONE', ( #12046, #14211, #7034, #9793, #8949, #8943 ) ) ;
#5773 = CARTESIAN_POINT ( 'NONE',  ( 0.1749999999999999889, 9.500000000000000000, 1.600000000000000089 ) ) ;
#5774 = EDGE_CURVE ( 'NONE', #7292, #12458, #4895, .T. ) ;
#5775 = ORIENTED_EDGE ( 'NONE', *, *, #14930, .F. ) ;
#5776 = CARTESIAN_POINT ( 'NONE',  ( 2.353343516942209668, -3.826605122864669362, 4.722803042560139275 ) ) ;
#5777 = CARTESIAN_POINT ( 'NONE',  ( 0.000000000000000000, 0.000000000000000000, 0.000000000000000000 ) ) ;
#5778 = CARTESIAN_POINT ( 'NONE',  ( -2.484260633728970546, -5.542161016949150643, 3.766563288620799366 ) ) ;
#5779 = ORIENTED_EDGE ( 'NONE', *, *, #17063, .T. ) ;
#5780 = CARTESIAN_POINT ( 'NONE',  ( 2.116444151961470066, -0.3533898305084750002, 3.670839500609349937 ) ) ;
#5781 = VERTEX_POINT ( 'NONE', #843 ) ;
#5782 = DIRECTION ( 'NONE',  ( 1.000000000000000000, 0.000000000000000000, -7.273661547324610053E-16 ) ) ;
#5783 = CARTESIAN_POINT ( 'NONE',  ( -1.750000000000000000, 11.40000000000000036, 7.550000000000000711 ) ) ;
#5784 = CARTESIAN_POINT ( 'NONE',  ( 1.985741519624368845, -2.495331814072259569, 4.178720363079467148 ) ) ;
#5785 = ORIENTED_EDGE ( 'NONE', *, *, #10780, .T. ) ;
#5786 = DIRECTION ( 'NONE',  ( -1.000000000000000000, 0.000000000000000000, 0.000000000000000000 ) ) ;
#5787 = PLANE ( 'NONE',  #7938 ) ;
#5788 = CARTESIAN_POINT ( 'NONE',  ( 1.351903350398191206, -0.4156779661016956062, 6.245004350000406212 ) ) ;
#5789 = ORIENTED_EDGE ( 'NONE', *, *, #7553, .T. ) ;
#5790 = DIRECTION ( 'NONE',  ( 2.379049338482479710E-16, 0.000000000000000000, 1.000000000000000000 ) ) ;
#5791 = CARTESIAN_POINT ( 'NONE',  ( -1.042222075699109407, -5.475423728813556323, 6.468743694056166227 ) ) ;
#5792 = AXIS2_PLACEMENT_3D ( 'NONE', #9744, #11223, #12605 ) ;
#5793 = ADVANCED_FACE ( 'NONE', ( #14718 ), #3609, .T. ) ;
#5794 = CARTESIAN_POINT ( 'NONE',  ( 2.088297318559229065, -0.09788135593220401165, 5.785136623276630807 ) ) ;
#5795 = ORIENTED_EDGE ( 'NONE', *, *, #7900, .T. ) ;
#5796 = LINE ( 'NONE', #11440, #17335 ) ;
#5797 = CARTESIAN_POINT ( 'NONE',  ( 2.326448859701049976, -2.219713230972780060, 4.344498395672269808 ) ) ;
#5798 = CARTESIAN_POINT ( 'NONE',  ( 1.800000000000000044, 11.40000000000000036, 7.649999999999999467 ) ) ;
#5799 = CARTESIAN_POINT ( 'NONE',  ( 1.937109463115360253, -2.173136654396201184, 4.019920026366761157 ) ) ;
#5800 = CARTESIAN_POINT ( 'NONE',  ( 0.5500000000000000444, 0.5999999999999999778, 3.299999999999999822 ) ) ;
#5801 = VERTEX_POINT ( 'NONE', #10453 ) ;
#5802 = DIRECTION ( 'NONE',  ( 1.480297366166869931E-15, 1.000000000000000000, -1.314768175368350090E-30 ) ) ;
#5803 = CARTESIAN_POINT ( 'NONE',  ( -2.058670345754650022, -0.5491525423728820243, 3.559656372813929881 ) ) ;
#5804 = CARTESIAN_POINT ( 'NONE',  ( 2.354888465609351389, -0.3978813559322044724, 5.923664702843856489 ) ) ;
#5805 = CARTESIAN_POINT ( 'NONE',  ( -0.9485663501270049647, -3.054250732991179440, 6.853826262002260528 ) ) ;
#5806 = CARTESIAN_POINT ( 'NONE',  ( -1.250000000000000000, 3.881370849898470254, 5.100000000000000533 ) ) ;
#5807 = CARTESIAN_POINT ( 'NONE',  ( -2.500000000000000000, 10.00000000000000000, 5.075305255429290705E-16 ) ) ;
#5808 = CARTESIAN_POINT ( 'NONE',  ( 2.332582362116870200, -5.068644067796610031, 4.387643303570810005 ) ) ;
#5809 = ORIENTED_EDGE ( 'NONE', *, *, #3144, .T. ) ;
#5810 = ORIENTED_EDGE ( 'NONE', *, *, #10528, .F. ) ;
#5811 = CARTESIAN_POINT ( 'NONE',  ( 1.889999999999999902, 8.500000000000000000, 0.5999999999999999778 ) ) ;
#5812 = DIRECTION ( 'NONE',  ( 0.000000000000000000, 1.000000000000000000, -1.110223024625159745E-16 ) ) ;
#5813 = ORIENTED_EDGE ( 'NONE', *, *, #16510, .F. ) ;
#5814 = AXIS2_PLACEMENT_3D ( 'NONE', #18256, #9577, #13841 ) ;
#5815 = DIRECTION ( 'NONE',  ( 0.000000000000000000, -1.000000000000000000, 0.000000000000000000 ) ) ;
#5816 = CARTESIAN_POINT ( 'NONE',  ( -2.065623031241579977, -5.033755237495680213, 3.572193642975310279 ) ) ;
#5817 = CARTESIAN_POINT ( 'NONE',  ( 1.864786684738361178, -0.7952867690272208412, 2.817120744449660652 ) ) ;
#5818 = DIRECTION ( 'NONE',  ( -3.289549702593060178E-16, 1.000000000000000000, 0.000000000000000000 ) ) ;
#5819 = CARTESIAN_POINT ( 'NONE',  ( 2.326448859701049976, -2.219713230972780060, 4.344498395672269808 ) ) ;
#5820 = VECTOR ( 'NONE', #15634, 1000.000000000000000 ) ;
#5821 = CARTESIAN_POINT ( 'NONE',  ( -4.898587196589400133E-17, 6.700000000000000178, 6.599999999999999645 ) ) ;
#5822 = CARTESIAN_POINT ( 'NONE',  ( 1.991984774470479946, -3.985782264522710339, 3.446707398186009907 ) ) ;
#5823 = CARTESIAN_POINT ( 'NONE',  ( 0.000000000000000000, 0.000000000000000000, 5.100000000000000533 ) ) ;
#5824 = CARTESIAN_POINT ( 'NONE',  ( 1.372465729645801602, -4.335106588847043696, 6.226839763556046847 ) ) ;
#5825 = VECTOR ( 'NONE', #9882, 1000.000000000000000 ) ;
#5826 = LINE ( 'NONE', #6005, #4967 ) ;
#5827 = AXIS2_PLACEMENT_3D ( 'NONE', #14710, #3143, #9053 ) ;
#5828 = EDGE_LOOP ( 'NONE', ( #10663, #906, #17385, #17329 ) ) ;
#5829 = CARTESIAN_POINT ( 'NONE',  ( -0.009452110982655715157, -0.5998079552954631577, 2.649999999999998579 ) ) ;
#5830 = VERTEX_POINT ( 'NONE', #740 ) ;
#5831 = DIRECTION ( 'NONE',  ( 1.224646799147351975E-16, -1.000000000000000000, -6.123233995736789455E-17 ) ) ;
#5832 = VERTEX_POINT ( 'NONE', #3515 ) ;
#5833 = CIRCLE ( 'NONE', #1702, 1.016666666666670160 ) ;
#5834 = CARTESIAN_POINT ( 'NONE',  ( 0.5500000000000000444, 6.450000000000000178, 3.399999999999999911 ) ) ;
#5835 = COLOUR_RGB ( '', 0.40784314, 0.44705882, 0.49803922) ;
#5836 = CARTESIAN_POINT ( 'NONE',  ( 0.7982439214406963357, -5.430932203389830626, 6.591424794228156081 ) ) ;
#5837 = CARTESIAN_POINT ( 'NONE',  ( -2.445954350973251312, -2.941650167909708458, 5.729767452368195180 ) ) ;
#5838 = VECTOR ( 'NONE', #7920, 1000.000000000000000 ) ;
#5839 = PRESENTATION_STYLE_ASSIGNMENT (( #13060 ) ) ;
#5840 = AXIS2_PLACEMENT_3D ( 'NONE', #3022, #1897, #14581 ) ;
#5841 = CARTESIAN_POINT ( 'NONE',  ( 4.898587196589403214E-17, 3.581751045813930112, 7.700000000000000178 ) ) ;
#5842 = DIRECTION ( 'NONE',  ( -1.000000000000000000, 0.000000000000000000, 7.401486830834370362E-16 ) ) ;
#5843 = CARTESIAN_POINT ( 'NONE',  ( -1.676695548152530968, -4.829629811528105776, 2.630596693608521885 ) ) ;
#5844 = PLANE ( 'NONE',  #16799 ) ;
#5845 = CARTESIAN_POINT ( 'NONE',  ( 0.7500000000000000000, 6.450000000000000178, 2.699264068711930253 ) ) ;
#5846 = CARTESIAN_POINT ( 'NONE',  ( 2.352760675243219968, -2.565196678937129882, 4.757121734156020132 ) ) ;
#5847 = VECTOR ( 'NONE', #15866, 1000.000000000000000 ) ;
#5848 = CARTESIAN_POINT ( 'NONE',  ( 1.919159680931818990, -3.733451969711523155, 3.970803207828129455 ) ) ;
#5849 = ADVANCED_FACE ( 'NONE', ( #9258 ), #8809, .T. ) ;
#5850 = VECTOR ( 'NONE', #5960, 1000.000000000000000 ) ;
#5851 = CARTESIAN_POINT ( 'NONE',  ( -1.943632316591239917, -0.2536016949152539723, 3.373048379518170048 ) ) ;
#5852 = CARTESIAN_POINT ( 'NONE',  ( 1.978267656359410154, -0.4023305084745769644, 5.974740860598790171 ) ) ;
#5853 = CARTESIAN_POINT ( 'NONE',  ( -1.899999999999999911, 0.5999999999999999778, 0.5999999999999999778 ) ) ;
#5854 = ADVANCED_FACE ( 'NONE', ( #5004 ), #6287, .T. ) ;
#5855 = ADVANCED_FACE ( 'NONE', ( #11777 ), #12042, .T. ) ;
#5856 = DIRECTION ( 'NONE',  ( 1.000000000000000000, 0.000000000000000000, 0.000000000000000000 ) ) ;
#5857 = VERTEX_POINT ( 'NONE', #9344 ) ;
#5858 = AXIS2_PLACEMENT_3D ( 'NONE', #16538, #10598, #3846 ) ;
#5859 = CARTESIAN_POINT ( 'NONE',  ( 0.5889081234606849957, -0.1379237288135600203, 6.978529000034869867 ) ) ;
#5860 = CARTESIAN_POINT ( 'NONE',  ( -1.854177340199669954, -1.610376859117309989, 6.149404042554720284 ) ) ;
#5861 = VERTEX_POINT ( 'NONE', #8979 ) ;
#5862 = ORIENTED_EDGE ( 'NONE', *, *, #2122, .T. ) ;
#5863 = CARTESIAN_POINT ( 'NONE',  ( 2.199335452462551022, -3.733451969711521379, 3.862342996790889771 ) ) ;
#5864 = CARTESIAN_POINT ( 'NONE',  ( -2.614198783383141045, -5.233262711864406391, 4.243032045539295360 ) ) ;
#5865 = VECTOR ( 'NONE', #12316, 1000.000000000000000 ) ;
#5866 = VECTOR ( 'NONE', #83, 1000.000000000000000 ) ;
#5867 = ORIENTED_EDGE ( 'NONE', *, *, #4426, .F. ) ;
#5868 = CARTESIAN_POINT ( 'NONE',  ( 1.725722849164588624, -0.4023305084745772420, 5.812007984777676661 ) ) ;
#5869 = EDGE_LOOP ( 'NONE', ( #14647, #12636, #10339, #11822 ) ) ;
#5870 = VECTOR ( 'NONE', #5404, 1000.000000000000000 ) ;
#5871 = EDGE_CURVE ( 'NONE', #17998, #8948, #13525, .T. ) ;
#5872 = CARTESIAN_POINT ( 'NONE',  ( -0.5999999999999999778, 11.40000000000000036, 7.599999999999999645 ) ) ;
#5873 = DIRECTION ( 'NONE',  ( 0.000000000000000000, 1.000000000000000000, 1.295260195396020040E-15 ) ) ;
#5874 = CARTESIAN_POINT ( 'NONE',  ( 1.472933559740161602, -2.751502985243430288, 6.130163826706326091 ) ) ;
#5876 = EDGE_CURVE ( 'NONE', #1173, #3985, #3696, .T. ) ;
#5875 = DIRECTION ( 'NONE',  ( 2.220446049250309876E-16, -1.000000000000000000, 0.000000000000000000 ) ) ;
#5877 = ORIENTED_EDGE ( 'NONE', *, *, #14281, .F. ) ;
#5878 = EDGE_CURVE ( 'NONE', #3985, #5295, #7594, .T. ) ;
#5879 = AXIS2_PLACEMENT_3D ( 'NONE', #2407, #16459, #13696 ) ;
#5880 = DIRECTION ( 'NONE',  ( -1.224646799147341867E-16, -1.000000000000000000, 0.000000000000000000 ) ) ;
#5881 = VECTOR ( 'NONE', #9533, 1000.000000000000000 ) ;
#5882 = CARTESIAN_POINT ( 'NONE',  ( 0.8731223871105069367, -0.4290254237288141370, 6.558046933601105799 ) ) ;
#5883 = ORIENTED_EDGE ( 'NONE', *, *, #10606, .T. ) ;
#5884 = CARTESIAN_POINT ( 'NONE',  ( -0.7476103186298618253, -5.582203389830510787, 2.787995836256459636 ) ) ;
#5885 = AXIS2_PLACEMENT_3D ( 'NONE', #5777, #17310, #12992 ) ;
#5886 = CARTESIAN_POINT ( 'NONE',  ( -0.4974685680287777023, -0.1601694915254239793, 7.000224381598740386 ) ) ;
#5887 = CARTESIAN_POINT ( 'NONE',  ( -3.766169468773179610E-15, -5.599999999999999645, 2.349999999999999645 ) ) ;
#5888 = VERTEX_POINT ( 'NONE', #2136 ) ;
#5889 = DIRECTION ( 'NONE',  ( 0.000000000000000000, 0.000000000000000000, 1.000000000000000000 ) ) ;
#5890 = VECTOR ( 'NONE', #9313, 1000.000000000000000 ) ;
#5891 = CARTESIAN_POINT ( 'NONE',  ( -1.571912189623050127, -1.264893411152959946, 6.451524409078659872 ) ) ;
#5892 = LINE ( 'NONE', #5798, #13536 ) ;
#5893 = CARTESIAN_POINT ( 'NONE',  ( -0.1526488871098711508, -1.847100618360169699, 2.652660223633551251 ) ) ;
#5895 = EDGE_CURVE ( 'NONE', #13769, #8163, #14626, .T. ) ;
#5894 = LINE ( 'NONE', #1733, #6413 ) ;
#5896 = ORIENTED_EDGE ( 'NONE', *, *, #4250, .T. ) ;
#5897 = FACE_BOUND ( 'NONE', #4279, .T. ) ;
#5898 = CARTESIAN_POINT ( 'NONE',  ( -1.666450993087168930, -0.4824152542372879826, 6.765380371283871597 ) ) ;
#5899 = AXIS2_PLACEMENT_3D ( 'NONE', #6708, #12365, #2739 ) ;
#5900 = CARTESIAN_POINT ( 'NONE',  ( -1.626408692231610109, -4.707719201459649838, 6.401040991074980369 ) ) ;
#5901 = DIRECTION ( 'NONE',  ( 0.000000000000000000, 0.000000000000000000, -1.000000000000000000 ) ) ;
#5902 = EDGE_CURVE ( 'NONE', #2720, #4993, #4719, .T. ) ;
#5903 = CARTESIAN_POINT ( 'NONE',  ( -1.000000000000000000, 5.400000000000000355, 7.700000000000000178 ) ) ;
#5904 = CARTESIAN_POINT ( 'NONE',  ( -2.653602652190420574, -5.224364406779660186, 4.735326402787099376 ) ) ;
#5905 = ORIENTED_EDGE ( 'NONE', *, *, #10853, .T. ) ;
#5906 = EDGE_LOOP ( 'NONE', ( #6619, #6176, #9363, #12869 ) ) ;
#5907 = LINE ( 'NONE', #10236, #8605 ) ;
#5908 = DIRECTION ( 'NONE',  ( 1.000000000000000000, 0.000000000000000000, -6.123233995736769734E-17 ) ) ;
#5909 = VERTEX_POINT ( 'NONE', #16034 ) ;
#5910 = EDGE_CURVE ( 'NONE', #16761, #1744, #1941, .T. ) ;
#5911 = CARTESIAN_POINT ( 'NONE',  ( -1.722199153441400066, -5.095857339597789526, 3.099360556065549943 ) ) ;
#5912 = APPLICATION_CONTEXT ( 'automotive_design' ) ;
#5913 = CARTESIAN_POINT ( 'NONE',  ( 0.2751970330256541808, -0.3251990024832501214, 2.050771348498781066 ) ) ;
#5914 = CARTESIAN_POINT ( 'NONE',  ( -1.800000000000000044, 0.5999999999999999778, 6.599999999999999645 ) ) ;
#5915 = CIRCLE ( 'NONE', #14770, 0.2500000000000002220 ) ;
#5916 = CARTESIAN_POINT ( 'NONE',  ( 1.332058588847409908, -2.499172690432239996, 6.640197310420189680 ) ) ;
#5918 = EDGE_CURVE ( 'NONE', #8572, #14730, #13336, .T. ) ;
#5917 = LINE ( 'NONE', #363, #8489 ) ;
#5919 = CARTESIAN_POINT ( 'NONE',  ( -2.461935615161759294, -1.680241723982170754, 5.690952430644365734 ) ) ;
#5920 = DIRECTION ( 'NONE',  ( 1.000000000000000000, 9.028005242978079560E-48, -6.123233995736769734E-17 ) ) ;
#5921 = CARTESIAN_POINT ( 'NONE',  ( -1.703239418290670049, -5.057043525783965876, 3.553755118148739900 ) ) ;
#5922 = PLANE ( 'NONE',  #256 ) ;
#5923 = DIRECTION ( 'NONE',  ( -6.123233995736769734E-17, -8.820551857043939970E-15, -1.000000000000000000 ) ) ;
#5924 = ORIENTED_EDGE ( 'NONE', *, *, #16405, .T. ) ;
#5925 = LINE ( 'NONE', #13141, #5752 ) ;
#5926 = ORIENTED_EDGE ( 'NONE', *, *, #11294, .T. ) ;
#5927 = VECTOR ( 'NONE', #15248, 1000.000000000000000 ) ;
#5928 = DIRECTION ( 'NONE',  ( 4.440892098500630106E-16, 4.440892098500630106E-16, -1.000000000000000000 ) ) ;
#5929 = VERTEX_POINT ( 'NONE', #17762 ) ;
#5930 = CARTESIAN_POINT ( 'NONE',  ( 0.05465110135556765225, -5.448728813559320372, 6.752241303418941243 ) ) ;
#5931 = CARTESIAN_POINT ( 'NONE',  ( -2.635341251434490495, -3.011515032774579215, 5.013193520829514860 ) ) ;
#5932 = SHAPE_REPRESENTATION ( 'Insulating Base Plate', ( #17681 ), #11500 ) ;
#5933 = DIRECTION ( 'NONE',  ( 1.632680918566409751E-16, -1.000000000000000000, -1.306144734853129823E-16 ) ) ;
#5934 = FACE_BOUND ( 'NONE', #12960, .T. ) ;
#5935 = DIRECTION ( 'NONE',  ( 0.000000000000000000, -1.000000000000000000, -1.306144734853123906E-16 ) ) ;
#5936 = DIRECTION ( 'NONE',  ( -1.000000000000000000, 6.161988852941170860E-64, 6.123233995736769734E-17 ) ) ;
#5937 = VECTOR ( 'NONE', #10340, 1000.000000000000000 ) ;
#5938 = CARTESIAN_POINT ( 'NONE',  ( 1.611907055891590002, -2.355602084342530045, 2.985210995296850189 ) ) ;
#5939 = CARTESIAN_POINT ( 'NONE',  ( 1.566607907718229553, -1.167899381639830203, 6.026891670824254810 ) ) ;
#5940 = CARTESIAN_POINT ( 'NONE',  ( -0.06264882350515391107, -0.1512711864406779960, 7.052569299041220319 ) ) ;
#5941 = CARTESIAN_POINT ( 'NONE',  ( 0.007887181101543709258, -5.024994858181869972, 2.435887274406050462 ) ) ;
#5942 = EDGE_CURVE ( 'NONE', #13228, #6816, #3412, .T. ) ;
#5943 = CARTESIAN_POINT ( 'NONE',  ( -0.9000000000000000222, 6.450000000000000178, 3.600000000000000089 ) ) ;
#5944 = ORIENTED_EDGE ( 'NONE', *, *, #1495, .T. ) ;
#5945 = CARTESIAN_POINT ( 'NONE',  ( 2.235075160050071119, -3.966334852594401994, 6.130927224539736820 ) ) ;
#5946 = CARTESIAN_POINT ( 'NONE',  ( -1.449568901432419343, -0.2625000000000002331, 3.250431098567584165 ) ) ;
#5947 = CARTESIAN_POINT ( 'NONE',  ( -2.005512128484160161, -1.913124606865060029, 3.468469736471389897 ) ) ;
#5948 = ORIENTED_EDGE ( 'NONE', *, *, #10412, .T. ) ;
#5949 = PLANE ( 'NONE',  #847 ) ;
#5950 = ORIENTED_EDGE ( 'NONE', *, *, #17100, .F. ) ;
#5951 = CARTESIAN_POINT ( 'NONE',  ( -2.322440385110939864, -3.081379897639439758, 4.319189883157441123 ) ) ;
#5952 = DIRECTION ( 'NONE',  ( 1.000000000000000000, 0.000000000000000000, 0.000000000000000000 ) ) ;
#5953 = CARTESIAN_POINT ( 'NONE',  ( -0.08231150243516484333, -5.598516949152545941, 2.050000000000001155 ) ) ;
#5954 = VERTEX_POINT ( 'NONE', #8075 ) ;
#5955 = FACE_OUTER_BOUND ( 'NONE', #13234, .T. ) ;
#5956 = EDGE_CURVE ( 'NONE', #15379, #7912, #3891, .T. ) ;
#5957 = CARTESIAN_POINT ( 'NONE',  ( -2.234315482767910144, -0.5402542372881360411, 3.960850823455329905 ) ) ;
#5958 = ORIENTED_EDGE ( 'NONE', *, *, #2102, .F. ) ;
#5959 = CARTESIAN_POINT ( 'NONE',  ( -0.6628679656440369383, 6.450000000000000178, 1.670710678118660031 ) ) ;
#5960 = DIRECTION ( 'NONE',  ( 0.000000000000000000, 0.000000000000000000, 1.000000000000000000 ) ) ;
#5961 = CARTESIAN_POINT ( 'NONE',  ( 1.333132471082870918, -2.774791273531719060, 6.261300629978916454 ) ) ;
#5962 = ORIENTED_EDGE ( 'NONE', *, *, #6088, .F. ) ;
#5963 = DIRECTION ( 'NONE',  ( -1.000000000000000000, 0.000000000000000000, 0.000000000000000000 ) ) ;
#5964 = DIRECTION ( 'NONE',  ( 0.000000000000000000, -1.000000000000000000, 0.000000000000000000 ) ) ;
#5965 = CARTESIAN_POINT ( 'NONE',  ( -1.000000000000000000, -5.599999999999999645, 3.673738709727309981 ) ) ;
#5966 = ORIENTED_EDGE ( 'NONE', *, *, #13240, .F. ) ;
#5967 = DIRECTION ( 'NONE',  ( 1.000000000000000000, 0.000000000000000000, 0.000000000000000000 ) ) ;
#5968 = CARTESIAN_POINT ( 'NONE',  ( -1.725722849164588624, -5.497669491525425833, 5.812007984777676661 ) ) ;
#5969 = ADVANCED_FACE ( 'NONE', ( #6576 ), #6941, .T. ) ;
#5970 = FACE_OUTER_BOUND ( 'NONE', #15749, .T. ) ;
#5971 = EDGE_CURVE ( 'NONE', #9567, #5409, #12324, .T. ) ;
#5972 = CARTESIAN_POINT ( 'NONE',  ( 2.549960444629811640, -4.055647129387581984, 3.964598460822105874 ) ) ;
#5973 = VERTEX_POINT ( 'NONE', #13894 ) ;
#5974 = EDGE_CURVE ( 'NONE', #3213, #11589, #6666, .T. ) ;
#5975 = CARTESIAN_POINT ( 'NONE',  ( -1.021156010535440029, -1.753947465207009948, 2.579625955254300163 ) ) ;
#5976 = EDGE_CURVE ( 'NONE', #3272, #13978, #1297, .T. ) ;
#5977 = PLANE ( 'NONE',  #819 ) ;
#5978 = ADVANCED_FACE ( 'NONE', ( #17943 ), #1029, .T. ) ;
#5979 = CARTESIAN_POINT ( 'NONE',  ( 1.777111910197639810, -2.126560077819629413, 3.672004328189181432 ) ) ;
#5980 = DIRECTION ( 'NONE',  ( 0.000000000000000000, -1.000000000000000000, 0.000000000000000000 ) ) ;
#5981 = DIRECTION ( 'NONE',  ( -1.224646799147350002E-16, 1.000000000000000000, 6.123233995736759873E-17 ) ) ;
#5982 = ORIENTED_EDGE ( 'NONE', *, *, #1114, .T. ) ;
#5983 = CARTESIAN_POINT ( 'NONE',  ( 0.5291502622129179434, 0.1000000000000000056, 7.700000000000000178 ) ) ;
#5984 = CARTESIAN_POINT ( 'NONE',  ( 2.589817782457058737, -0.6361096273691766445, 4.120381550729950604 ) ) ;
#5985 = AXIS2_PLACEMENT_3D ( 'NONE', #16537, #15342, #8112 ) ;
#5986 = VECTOR ( 'NONE', #1160, 1000.000000000000000 ) ;
#5987 = CARTESIAN_POINT ( 'NONE',  ( -1.460675875430050175, -4.684430913171359734, 6.545310725710059785 ) ) ;
#5988 = DIRECTION ( 'NONE',  ( 1.000000000000000000, -1.224646799147350002E-16, 0.000000000000000000 ) ) ;
#5989 = CARTESIAN_POINT ( 'NONE',  ( -1.889999999999999902, 7.900000000000000355, 0.5999999999999999778 ) ) ;
#5990 = CARTESIAN_POINT ( 'NONE',  ( -2.087380238839969593, -5.193220338983044471, 6.338810156469112833 ) ) ;
#5991 = VERTEX_POINT ( 'NONE', #13977 ) ;
#5992 = ORIENTED_EDGE ( 'NONE', *, *, #15088, .T. ) ;
#5993 = PLANE ( 'NONE',  #15117 ) ;
#5994 = DIRECTION ( 'NONE',  ( 0.000000000000000000, 0.000000000000000000, 1.000000000000000000 ) ) ;
#5995 = ADVANCED_FACE ( 'NONE', ( #10939 ), #10837, .F. ) ;
#5996 = EDGE_LOOP ( 'NONE', ( #437, #17057, #17511, #12351 ) ) ;
#5997 = CARTESIAN_POINT ( 'NONE',  ( 2.651429253058529945, -0.9815930753335269099, 4.585822029124893895 ) ) ;
#5998 = CARTESIAN_POINT ( 'NONE',  ( -0.009452110982655099330, -0.5998079552954631577, 2.649999999999998579 ) ) ;
#5999 = CARTESIAN_POINT ( 'NONE',  ( 1.250000000000000000, 0.5999999999999999778, 6.100000000000000533 ) ) ;
#6000 = CARTESIAN_POINT ( 'NONE',  ( 1.948278411993589865, -2.406019537279080467, 6.020210936496000365 ) ) ;
#6001 = DIRECTION ( 'NONE',  ( -1.000000000000000000, 1.153478467143200106E-14, -8.997169018144999103E-17 ) ) ;
#6002 = CARTESIAN_POINT ( 'NONE',  ( -0.4247583764260595141, -1.424070552811000701, 7.319674410047512403 ) ) ;
#6003 = DIRECTION ( 'NONE',  ( 1.908195823574489776E-16, -1.000000000000000000, -1.387778780781449866E-16 ) ) ;
#6004 = CARTESIAN_POINT ( 'NONE',  ( -1.117157304995339606, -4.661142624883069630, 6.422457952614126775 ) ) ;
#6005 = CARTESIAN_POINT ( 'NONE',  ( 1.899999999999999911, 11.15000000000000036, -3.616154994493369454E-16 ) ) ;
#6006 = CARTESIAN_POINT ( 'NONE',  ( 2.270487904532159984, -0.3622881355932209835, 4.080813552109670894 ) ) ;
#6007 = CARTESIAN_POINT ( 'NONE',  ( 2.500000000000000000, 2.799999999999999822, 1.600000000000000089 ) ) ;
#6008 = VERTEX_POINT ( 'NONE', #16483 ) ;
#6009 = STYLED_ITEM ( 'NONE', ( #5385 ), #1876 ) ;
#6010 = CARTESIAN_POINT ( 'NONE',  ( -1.875000000000000000, 11.25000000000000000, 7.700000000000000178 ) ) ;
#6011 = ORIENTED_EDGE ( 'NONE', *, *, #324, .T. ) ;
#6012 = DIRECTION ( 'NONE',  ( -3.700743415417179758E-16, -1.000000000000000000, -1.665334536937730077E-15 ) ) ;
#6013 = CARTESIAN_POINT ( 'NONE',  ( -1.289999999999999813, 7.900000000000014566, 4.318333862165718414E-15 ) ) ;
#6014 = EDGE_CURVE ( 'NONE', #14398, #1432, #8157, .T. ) ;
#6015 = ORIENTED_EDGE ( 'NONE', *, *, #2087, .F. ) ;
#6016 = CARTESIAN_POINT ( 'NONE',  ( -1.614765845140348821, -5.493220338983046069, 5.967758800287426446 ) ) ;
#6017 = CARTESIAN_POINT ( 'NONE',  ( 1.836970198721020197E-17, 2.600000000000000089, 7.700000000000000178 ) ) ;
#6018 = CARTESIAN_POINT ( 'NONE',  ( 0.7137241095604313079, -3.500569086828633658, 2.143887406933319362 ) ) ;
#6019 = SURFACE_STYLE_FILL_AREA ( #8708 ) ;
#6020 =( LENGTH_UNIT ( ) NAMED_UNIT ( * ) SI_UNIT ( .MILLI., .METRE. ) );
#6021 = AXIS2_PLACEMENT_3D ( 'NONE', #2696, #11303, #14178 ) ;
#6022 = DIRECTION ( 'NONE',  ( 0.000000000000000000, 0.000000000000000000, 1.000000000000000000 ) ) ;
#6023 = CARTESIAN_POINT ( 'NONE',  ( -0.1569242594330230167, -1.400782264522720144, 7.048216443236290374 ) ) ;
#6024 = DIRECTION ( 'NONE',  ( 0.000000000000000000, 1.000000000000000000, 2.220446049250309876E-16 ) ) ;
#6025 = CARTESIAN_POINT ( 'NONE',  ( -1.914021115237000137, -4.754295778036220277, 6.069404563272239983 ) ) ;
#6026 = CARTESIAN_POINT ( 'NONE',  ( -1.436030008293460503, -4.408812330071866015, 6.167214932417466322 ) ) ;
#6027 = CARTESIAN_POINT ( 'NONE',  ( 0.001589539283869510202, -5.124807148327449546, 2.499688892524289496 ) ) ;
#6028 = ORIENTED_EDGE ( 'NONE', *, *, #741, .F. ) ;
#6029 = CARTESIAN_POINT ( 'NONE',  ( 0.9038768003982520227, -4.129352870612409632, 7.195219513931331967 ) ) ;
#6030 = CARTESIAN_POINT ( 'NONE',  ( 2.046424002475610404, -0.07118644067796651986, 4.536201610417760044 ) ) ;
#6031 = CARTESIAN_POINT ( 'NONE',  ( 2.337178851518220135, -2.588484967225419986, 4.976298214796759822 ) ) ;
#6032 = VECTOR ( 'NONE', #14901, 1000.000000000000000 ) ;
#6033 = ORIENTED_EDGE ( 'NONE', *, *, #8895, .F. ) ;
#6034 = ORIENTED_EDGE ( 'NONE', *, *, #17646, .F. ) ;
#6035 = DIRECTION ( 'NONE',  ( -6.049014748177260544E-16, 2.493473113004675144E-16, -1.000000000000000000 ) ) ;
#6036 = VERTEX_POINT ( 'NONE', #11106 ) ;
#6037 = CARTESIAN_POINT ( 'NONE',  ( -0.9170541073686518940, -4.315659176918721585, 6.867431071947199150 ) ) ;
#6038 = APPLICATION_PROTOCOL_DEFINITION ( 'draft international standard', 'automotive_design', 1998, #10645 ) ;
#6039 = CARTESIAN_POINT ( 'NONE',  ( 2.304156201936080617, -5.099788135593215976, 6.016707707703351282 ) ) ;
#6040 = EDGE_LOOP ( 'NONE', ( #12850, #3981, #13950, #18004, #6655, #4397, #3929, #130, #9619, #7782, #13883, #16137, #1338, #4654, #1868, #13602, #3878, #10188 ) ) ;
#6041 = CARTESIAN_POINT ( 'NONE',  ( 8.549934884138839976E-16, 6.262741699796950279, 5.100000000000000533 ) ) ;
#6042 = CARTESIAN_POINT ( 'NONE',  ( 2.353194804772640314, -0.3756355932203400139, 4.731327187377229571 ) ) ;
#6043 = VERTEX_POINT ( 'NONE', #5467 ) ;
#6044 = CARTESIAN_POINT ( 'NONE',  ( 0.1749999999999999889, 4.299999999999999822, 1.600000000000000089 ) ) ;
#6045 = DIRECTION ( 'NONE',  ( -1.000000000000000000, 0.000000000000000000, 0.000000000000000000 ) ) ;
#6046 = AXIS2_PLACEMENT_3D ( 'NONE', #13780, #2580, #5272 ) ;
#6047 = CARTESIAN_POINT ( 'NONE',  ( -2.029711248330079876, -3.380286769027221805, 4.391497016172549728 ) ) ;
#6048 = CARTESIAN_POINT ( 'NONE',  ( 2.386628511786341722, -0.05338983050847501133, 3.539457309197775459 ) ) ;
#6049 = VERTEX_POINT ( 'NONE', #3801 ) ;
#6050 = DIRECTION ( 'NONE',  ( -1.000000000000000000, 1.668003342285391304E-16, 0.000000000000000000 ) ) ;
#6051 = EDGE_LOOP ( 'NONE', ( #2060, #5443, #2855, #591 ) ) ;
#6052 = CARTESIAN_POINT ( 'NONE',  ( -0.5500000000000000444, 6.450000000000000178, 3.299999999999999822 ) ) ;
#6053 = CARTESIAN_POINT ( 'NONE',  ( 0.4339619423229844619, -5.439830508474575943, 6.706578715862737461 ) ) ;
#6054 = LINE ( 'NONE', #6147, #331 ) ;
#6055 = CARTESIAN_POINT ( 'NONE',  ( -2.623186471072040504, -3.380286769027221805, 4.297499775172091141 ) ) ;
#6056 = ORIENTED_EDGE ( 'NONE', *, *, #754, .T. ) ;
#6057 = CARTESIAN_POINT ( 'NONE',  ( 2.351999299633229956, -2.266289807549350055, 4.782734406438239994 ) ) ;
#6058 = CARTESIAN_POINT ( 'NONE',  ( -1.300000000000000044, 1.592040838891560081E-16, 7.599999999999999645 ) ) ;
#6059 = LINE ( 'NONE', #3291, #1635 ) ;
#6060 = CARTESIAN_POINT ( 'NONE',  ( 0.4194839839381755975, -1.916965483225031130, 2.690289814463930895 ) ) ;
#6061 = CARTESIAN_POINT ( 'NONE',  ( -1.899999999999999911, 4.700000000000000178, 1.600000000000000089 ) ) ;
#6062 = FACE_OUTER_BOUND ( 'NONE', #1193, .T. ) ;
#6063 = ORIENTED_EDGE ( 'NONE', *, *, #1894, .F. ) ;
#6064 = CARTESIAN_POINT ( 'NONE',  ( -0.7500000000000000000, 3.050000000000000266, 3.200000000000000178 ) ) ;
#6065 = VECTOR ( 'NONE', #11035, 1000.000000000000000 ) ;
#6066 = EDGE_CURVE ( 'NONE', #4195, #8282, #8529, .T. ) ;
#6067 = DIRECTION ( 'NONE',  ( 1.224646799147350002E-16, -1.000000000000000000, -6.123233995736769734E-17 ) ) ;
#6068 = CARTESIAN_POINT ( 'NONE',  ( -2.470260739716218179, -1.567641158900710430, 3.729986819255259878 ) ) ;
#6069 = ADVANCED_FACE ( 'NONE', ( #11021 ), #8343, .T. ) ;
#6070 = CARTESIAN_POINT ( 'NONE',  ( -0.4617942143426889690, -0.5906145504024210569, 2.383143958488499692 ) ) ;
#6071 = DIRECTION ( 'NONE',  ( -6.123233995736769734E-17, 3.749399456654650178E-33, -1.000000000000000000 ) ) ;
#6072 = EDGE_CURVE ( 'NONE', #4501, #18124, #9455, .T. ) ;
#6073 = DIRECTION ( 'NONE',  ( 0.000000000000000000, 1.000000000000000000, 0.000000000000000000 ) ) ;
#6074 = CARTESIAN_POINT ( 'NONE',  ( 2.143090896833110381, -5.095338983050850423, 5.672454929438339732 ) ) ;
#6075 = ORIENTED_EDGE ( 'NONE', *, *, #14817, .F. ) ;
#6076 = ORIENTED_EDGE ( 'NONE', *, *, #14476, .F. ) ;
#6077 = LINE ( 'NONE', #617, #17752 ) ;
#6078 =( LENGTH_UNIT ( ) NAMED_UNIT ( * ) SI_UNIT ( .MILLI., .METRE. ) );
#6079 = DIRECTION ( 'NONE',  ( 1.000000000000000000, 0.000000000000000000, -1.110223024625159992E-16 ) ) ;
#6080 = ORIENTED_EDGE ( 'NONE', *, *, #12799, .T. ) ;
#6081 = CARTESIAN_POINT ( 'NONE',  ( 1.899999999999999911, 11.29999999999999893, 7.649999999999999467 ) ) ;
#6082 = CARTESIAN_POINT ( 'NONE',  ( -2.612083973477999699, -1.819971453711898945, 4.230818789270855085 ) ) ;
#6083 = DIRECTION ( 'NONE',  ( 0.000000000000000000, 0.000000000000000000, -1.000000000000000000 ) ) ;
#6084 = PLANE ( 'NONE',  #5250 ) ;
#6085 = VECTOR ( 'NONE', #10933, 1000.000000000000000 ) ;
#6086 = CARTESIAN_POINT ( 'NONE',  ( 1.781655196750449921, -2.079983501243049648, 3.162323035427780482 ) ) ;
#6087 = CARTESIAN_POINT ( 'NONE',  ( 1.730954623551391736, -5.333856471231995577, 2.683219139909288842 ) ) ;
#6088 = EDGE_CURVE ( 'NONE', #7297, #14593, #7353, .T. ) ;
#6089 = CARTESIAN_POINT ( 'NONE',  ( -0.6672256841320821641, -1.447358841099289251, 7.268642361138727637 ) ) ;
#6090 = CARTESIAN_POINT ( 'NONE',  ( 1.889999999999999902, 7.299999999999999822, 0.6099999999999999867 ) ) ;
#6091 = CARTESIAN_POINT ( 'NONE',  ( -2.036910256464079971, -4.940602084342534894, 4.443293066459140128 ) ) ;
#6092 = EDGE_CURVE ( 'NONE', #3526, #17345, #11173, .T. ) ;
#6093 = PLANE ( 'NONE',  #7680 ) ;
#6094 = ORIENTED_EDGE ( 'NONE', *, *, #12109, .T. ) ;
#6095 = CARTESIAN_POINT ( 'NONE',  ( 0.5677251586959709551, -5.311531839079339790, 2.399563163165729929 ) ) ;
#6096 = ORIENTED_EDGE ( 'NONE', *, *, #13431, .T. ) ;
#6097 = DIRECTION ( 'NONE',  ( 6.123233995736769734E-17, 0.000000000000000000, 1.000000000000000000 ) ) ;
#6098 = FACE_OUTER_BOUND ( 'NONE', #17094, .T. ) ;
#6099 = ORIENTED_EDGE ( 'NONE', *, *, #18216, .T. ) ;
#6100 = FACE_OUTER_BOUND ( 'NONE', #10115, .T. ) ;
#6101 = CARTESIAN_POINT ( 'NONE',  ( 2.245209214543399945, -2.635061543801989981, 5.405536158119010004 ) ) ;
#6102 = PLANE ( 'NONE',  #14409 ) ;
#6103 = CARTESIAN_POINT ( 'NONE',  ( 2.332582362116870200, -5.368644067796609853, 4.387643303570810005 ) ) ;
#6104 = VECTOR ( 'NONE', #17124, 1000.000000000000000 ) ;
#6105 = LINE ( 'NONE', #11769, #16462 ) ;
#6106 = CIRCLE ( 'NONE', #1962, 0.2500000000000002220 ) ;
#6107 = CARTESIAN_POINT ( 'NONE',  ( -1.552749016687749783, -1.563800282540730002, 6.468535037441760061 ) ) ;
#6108 = EDGE_CURVE ( 'NONE', #4420, #1943, #2690, .T. ) ;
#6109 = CARTESIAN_POINT ( 'NONE',  ( -0.2620510901103649815, -3.706322805063249959, 2.361180871966390260 ) ) ;
#6110 = CARTESIAN_POINT ( 'NONE',  ( 1.876226141297899774, -0.8884399221803740421, 3.866526959224306115 ) ) ;
#6111 = ADVANCED_FACE ( 'NONE', ( #5561, #11208, #16852, #4161 ), #1490, .T. ) ;
#6112 = LINE ( 'NONE', #9060, #12355 ) ;
#6113 = CIRCLE ( 'NONE', #16520, 0.2000000000000000389 ) ;
#6114 = AXIS2_PLACEMENT_3D ( 'NONE', #13032, #7656, #3383 ) ;
#6115 = DIRECTION ( 'NONE',  ( 1.224646799147349263E-16, 0.000000000000000000, 1.000000000000000000 ) ) ;
#6116 = ORIENTED_EDGE ( 'NONE', *, *, #12874, .F. ) ;
#6117 = CARTESIAN_POINT ( 'NONE',  ( 0.7476103186298468373, -0.3177966101694921219, 2.787995836256459636 ) ) ;
#6118 = CARTESIAN_POINT ( 'NONE',  ( 0.1768565782245979934, -3.752899381639830168, 2.353200596935780098 ) ) ;
#6119 = VERTEX_POINT ( 'NONE', #4517 ) ;
#6120 = ORIENTED_EDGE ( 'NONE', *, *, #359, .T. ) ;
#6121 = FACE_OUTER_BOUND ( 'NONE', #10866, .T. ) ;
#6122 = AXIS2_PLACEMENT_3D ( 'NONE', #16534, #3842, #9198 ) ;
#6123 = ORIENTED_EDGE ( 'NONE', *, *, #8168, .F. ) ;
#6124 = AXIS2_PLACEMENT_3D ( 'NONE', #8655, #8840, #328 ) ;
#6125 = CARTESIAN_POINT ( 'NONE',  ( -0.06276132972181576453, -4.222506023765570937, 7.052616990284527709 ) ) ;
#6126 = SHAPE_DEFINITION_REPRESENTATION ( #6985, #16473 ) ;
#6127 = CARTESIAN_POINT ( 'NONE',  ( 2.650076489488250697, -5.077542372881359789, 4.841243018609314497 ) ) ;
#6128 = CARTESIAN_POINT ( 'NONE',  ( -1.875000000000000000, 2.296212748401290437E-16, 7.700000000000000178 ) ) ;
#6129 = CARTESIAN_POINT ( 'NONE',  ( -1.943632316591239917, -0.5536016949152539057, 3.373048379518170048 ) ) ;
#6130 = AXIS2_PLACEMENT_3D ( 'NONE', #14736, #8910, #17315 ) ;
#6131 = ORIENTED_EDGE ( 'NONE', *, *, #18056, .F. ) ;
#6132 = VECTOR ( 'NONE', #5485, 1000.000000000000000 ) ;
#6133 = EDGE_CURVE ( 'NONE', #1501, #17047, #2915, .T. ) ;
#6134 = DIRECTION ( 'NONE',  ( 3.861645303044030038E-16, 1.000000000000000000, 1.268826313857319964E-16 ) ) ;
#6135 = CARTESIAN_POINT ( 'NONE',  ( -1.279347147864589251, -3.566593075333521767, 3.094331068408299412 ) ) ;
#6136 = CARTESIAN_POINT ( 'NONE',  ( -2.651721837666119796, -0.5269067796610176213, 4.594045830208265180 ) ) ;
#6137 = EDGE_CURVE ( 'NONE', #7174, #2720, #1760, .T. ) ;
#6138 = AXIS2_PLACEMENT_3D ( 'NONE', #15526, #12639, #18264 ) ;
#6139 = VERTEX_POINT ( 'NONE', #11562 ) ;
#6140 = LINE ( 'NONE', #17425, #4051 ) ;
#6141 = EDGE_LOOP ( 'NONE', ( #10578, #8582, #7132, #10372 ) ) ;
#6143 = CIRCLE ( 'NONE', #17364, 0.1499999999999999667 ) ;
#6142 = AXIS2_PLACEMENT_3D ( 'NONE', #2126, #9249, #734 ) ;
#6144 = DIRECTION ( 'NONE',  ( -8.971499188890128802E-16, 4.485749594445070317E-16, -1.000000000000000000 ) ) ;
#6145 = CARTESIAN_POINT ( 'NONE',  ( -0.2189795514005259958, -5.595550847457629651, 2.356806637999020015 ) ) ;
#6146 = VECTOR ( 'NONE', #4598, 1000.000000000000000 ) ;
#6147 = CARTESIAN_POINT ( 'NONE',  ( 0.1749999999999999889, 7.700000000000000178, 1.600000000000000089 ) ) ;
#6148 = CARTESIAN_POINT ( 'NONE',  ( -0.4478021372196530070, -0.2909039927201509945, 2.380136890750930156 ) ) ;
#6149 = CARTESIAN_POINT ( 'NONE',  ( 1.576846334488021473, -3.892629111369556139, 2.565364356520400513 ) ) ;
#6150 = ORIENTED_EDGE ( 'NONE', *, *, #5168, .T. ) ;
#6151 = AXIS2_PLACEMENT_3D ( 'NONE', #10462, #9069, #5012 ) ;
#6152 = CARTESIAN_POINT ( 'NONE',  ( -1.074829861819750043, -3.314262780522330143, 2.606322265575609975 ) ) ;
#6153 = DIRECTION ( 'NONE',  ( 4.440892098500620245E-16, -3.700743415417219694E-16, 1.000000000000000000 ) ) ;
#6154 = CARTESIAN_POINT ( 'NONE',  ( -0.02999999999999400022, 12.00000000000000000, 7.649999999999999467 ) ) ;
#6155 = VECTOR ( 'NONE', #12932, 1000.000000000000000 ) ;
#6156 = CARTESIAN_POINT ( 'NONE',  ( 1.520647680314149541, -3.640298816558361406, 3.320676805464615633 ) ) ;
#6157 = STYLED_ITEM ( 'NONE', ( #14492 ), #8348 ) ;
#6158 = AXIS2_PLACEMENT_3D ( 'NONE', #2110, #4977, #4876 ) ;
#6159 = DIRECTION ( 'NONE',  ( 2.055968564120659776E-16, 1.000000000000000000, 0.000000000000000000 ) ) ;
#6160 = DIRECTION ( 'NONE',  ( 0.000000000000000000, -1.000000000000000000, -1.586032892321649771E-16 ) ) ;
#6161 = CARTESIAN_POINT ( 'NONE',  ( 0.7854158957161911925, -1.963542059801608897, 2.803154272645130618 ) ) ;
#6162 = ORIENTED_EDGE ( 'NONE', *, *, #215, .T. ) ;
#6163 = CARTESIAN_POINT ( 'NONE',  ( -0.1749999999999999889, 4.299999999999999822, 0.5999999999999999778 ) ) ;
#6164 = CARTESIAN_POINT ( 'NONE',  ( -2.642463257358080853, -1.451199717459271454, 4.945970783863430142 ) ) ;
#6165 = ORIENTED_EDGE ( 'NONE', *, *, #11335, .T. ) ;
#6166 = CARTESIAN_POINT ( 'NONE',  ( -0.009452110982655708218, -0.5998079552954630467, 2.350000000000000089 ) ) ;
#6167 = CARTESIAN_POINT ( 'NONE',  ( -1.899999999999999911, 7.299999999999999822, 0.5999999999999999778 ) ) ;
#6168 = DIRECTION ( 'NONE',  ( 1.306144734853129823E-16, -1.000000000000000000, 0.000000000000000000 ) ) ;
#6169 = EDGE_CURVE ( 'NONE', #5684, #9295, #5826, .T. ) ;
#6170 = CARTESIAN_POINT ( 'NONE',  ( -0.7983658734557950165, -5.166525423728809407, 6.913847129767330735 ) ) ;
#6171 = VERTEX_POINT ( 'NONE', #10003 ) ;
#6172 = ORIENTED_EDGE ( 'NONE', *, *, #15821, .T. ) ;
#6173 = CARTESIAN_POINT ( 'NONE',  ( 2.500000000000000000, 9.199999999999999289, 0.6099999999999999867 ) ) ;
#6174 =( NAMED_UNIT ( * ) SI_UNIT ( $, .STERADIAN. ) SOLID_ANGLE_UNIT ( ) );
#6175 = DIRECTION ( 'NONE',  ( -6.049014748177260544E-16, 0.000000000000000000, -1.000000000000000000 ) ) ;
#6176 = ORIENTED_EDGE ( 'NONE', *, *, #9764, .T. ) ;
#6177 = CARTESIAN_POINT ( 'NONE',  ( 1.213493134184789657, -2.285737219477670390, 2.339799138571409642 ) ) ;
#6178 = EDGE_CURVE ( 'NONE', #16414, #18253, #1580, .T. ) ;
#6179 = EDGE_CURVE ( 'NONE', #1946, #5569, #15553, .T. ) ;
#6180 = DIRECTION ( 'NONE',  ( 0.000000000000000000, 0.000000000000000000, 1.000000000000000000 ) ) ;
#6181 = DIRECTION ( 'NONE',  ( 0.000000000000000000, 0.000000000000000000, 1.000000000000000000 ) ) ;
#6182 = ADVANCED_FACE ( 'NONE', ( #2874 ), #10169, .F. ) ;
#6183 = CARTESIAN_POINT ( 'NONE',  ( 0.9485663501270550357, -2.545749267008810435, 6.853826262002240988 ) ) ;
#6184 = LINE ( 'NONE', #11840, #2873 ) ;
#6185 = CARTESIAN_POINT ( 'NONE',  ( 2.306572132003631648, -1.121322805063259542, 6.012569500204132389 ) ) ;
#6186 = CIRCLE ( 'NONE', #16549, 0.1000000000000000472 ) ;
#6187 = FACE_BOUND ( 'NONE', #10442, .T. ) ;
#6188 = CARTESIAN_POINT ( 'NONE',  ( 1.250000000000000000, 7.799999999999999822, 7.599999999999999645 ) ) ;
#6189 = EDGE_LOOP ( 'NONE', ( #17408, #12240, #16123, #8207 ) ) ;
#6190 = PRODUCT_DEFINITION_FORMATION_WITH_SPECIFIED_SOURCE ( 'ANY', '', #4881, .NOT_KNOWN. ) ;
#6191 = CARTESIAN_POINT ( 'NONE',  ( 7.069631497386979886E-16, 5.131370849898479136, 5.100000000000000533 ) ) ;
#6192 = ORIENTED_EDGE ( 'NONE', *, *, #6392, .T. ) ;
#6193 = PLANE ( 'NONE',  #2274 ) ;
#6194 = CARTESIAN_POINT ( 'NONE',  ( -1.875000000000000000, 0.7500000000000000000, 7.700000000000000178 ) ) ;
#6195 = EDGE_CURVE ( 'NONE', #7698, #796, #17019, .T. ) ;
#6196 = ORIENTED_EDGE ( 'NONE', *, *, #16146, .F. ) ;
#6197 = VECTOR ( 'NONE', #9039, 1000.000000000000000 ) ;
#6198 = DIRECTION ( 'NONE',  ( 0.000000000000000000, 1.000000000000000000, 0.000000000000000000 ) ) ;
#6199 = CARTESIAN_POINT ( 'NONE',  ( 1.265407828724300021, -2.309025507765960050, 2.715689360385540319 ) ) ;
#6200 = ADVANCED_FACE ( 'NONE', ( #283 ), #5922, .T. ) ;
#6201 = DIRECTION ( 'NONE',  ( -1.000000000000000000, 6.437450399132682577E-16, 0.000000000000000000 ) ) ;
#6202 = CARTESIAN_POINT ( 'NONE',  ( 1.694257473570984995, -0.4987256491549267312, 3.023551124676525426 ) ) ;
#6203 = ADVANCED_FACE ( 'NONE', ( #8523 ), #11476, .T. ) ;
#6204 = CARTESIAN_POINT ( 'NONE',  ( 8.416823969807580597E-17, 6.262741699796950279, 5.100000000000000533 ) ) ;
#6205 = ADVANCED_BREP_SHAPE_REPRESENTATION ( '', ( #7785, #17681 ), #5599 ) ;
#6206 = DIRECTION ( 'NONE',  ( 0.7071067811865470176, 9.235837992257496050E-17, -0.7071067811865480168 ) ) ;
#6207 = CARTESIAN_POINT ( 'NONE',  ( 0.8242394280877100021, -4.428259742000189902, 6.904399023015010073 ) ) ;
#6208 = CARTESIAN_POINT ( 'NONE',  ( 2.050563521385710075, -1.004881363621820567, 4.800454404529174823 ) ) ;
#6209 = DIRECTION ( 'NONE',  ( 2.220446049250309876E-16, 0.000000000000000000, -1.000000000000000000 ) ) ;
#6210 = VECTOR ( 'NONE', #5790, 1000.000000000000000 ) ;
#6211 = ORIENTED_EDGE ( 'NONE', *, *, #3226, .T. ) ;
#6212 = CARTESIAN_POINT ( 'NONE',  ( -1.880631435828179265, -0.2447033898305090438, 3.876649216148230437 ) ) ;
#6213 = CARTESIAN_POINT ( 'NONE',  ( 2.260890494820590124, -4.055647129387580208, 4.046455925041149371 ) ) ;
#6214 = VERTEX_POINT ( 'NONE', #14064 ) ;
#6215 = LINE ( 'NONE', #2045, #2921 ) ;
#6216 = EDGE_CURVE ( 'NONE', #4195, #2455, #10255, .T. ) ;
#6217 = ORIENTED_EDGE ( 'NONE', *, *, #10146, .T. ) ;
#6218 = DIRECTION ( 'NONE',  ( -7.401486830834380223E-16, -1.000000000000000000, 1.110223024625159992E-16 ) ) ;
#6219 = CARTESIAN_POINT ( 'NONE',  ( -2.386628511786350160, -5.246610169491530584, 3.539457309197792778 ) ) ;
#6220 = EDGE_CURVE ( 'NONE', #5991, #10145, #8697, .T. ) ;
#6221 = DIRECTION ( 'NONE',  ( 0.000000000000000000, -1.000000000000000000, -8.881784197001250351E-16 ) ) ;
#6222 = VECTOR ( 'NONE', #3438, 1000.000000000000000 ) ;
#6223 = CARTESIAN_POINT ( 'NONE',  ( 2.318251751302029984, -0.3667372881355940306, 4.294764266798990704 ) ) ;
#6224 = ORIENTED_EDGE ( 'NONE', *, *, #4183, .F. ) ;
#6225 = CARTESIAN_POINT ( 'NONE',  ( 1.912899118714319169, -4.218665147405596727, 5.445465495009710111 ) ) ;
#6226 = CARTESIAN_POINT ( 'NONE',  ( -0.3171869470818471370, -0.4557203389830515317, 7.334814496515233095 ) ) ;
#6227 = ORIENTED_EDGE ( 'NONE', *, *, #3392, .T. ) ;
#6228 = EDGE_CURVE ( 'NONE', #6669, #6864, #14174, .T. ) ;
#6229 = CARTESIAN_POINT ( 'NONE',  ( -1.467041701146829746, -0.4779661016949154906, 6.911479965439912831 ) ) ;
#6230 = ORIENTED_EDGE ( 'NONE', *, *, #10610, .T. ) ;
#6231 = VECTOR ( 'NONE', #10773, 1000.000000000000000 ) ;
#6232 = CARTESIAN_POINT ( 'NONE',  ( -2.500000000000000000, 10.00000000000000000, 0.5999999999999999778 ) ) ;
#6233 = CARTESIAN_POINT ( 'NONE',  ( 1.399999999999999911, -6.000000000000000000, 5.100000000000000533 ) ) ;
#6234 = CARTESIAN_POINT ( 'NONE',  ( -0.06264882350515386944, -0.1512711864406780238, 7.052569299041217654 ) ) ;
#6235 = CARTESIAN_POINT ( 'NONE',  ( 2.550815101416278541, -4.195376859117311064, 5.432431574543660879 ) ) ;
#6236 = EDGE_CURVE ( 'NONE', #12277, #9534, #7310, .T. ) ;
#6237 = ORIENTED_EDGE ( 'NONE', *, *, #1890, .T. ) ;
#6238 = CARTESIAN_POINT ( 'NONE',  ( -1.526791597786389953, -2.825208726468269926, 6.490992212270280781 ) ) ;
#6239 = CARTESIAN_POINT ( 'NONE',  ( -0.5500000000000000444, 6.450000000000000178, 2.699264068711930253 ) ) ;
#6240 = DIRECTION ( 'NONE',  ( -4.177994306516050823E-17, 0.7310552682428690385, -0.6823182503600111470 ) ) ;
#6241 = CARTESIAN_POINT ( 'NONE',  ( -0.5805547688319036004, -3.360839357098899693, 2.730772231808969774 ) ) ;
#6242 = LINE ( 'NONE', #974, #12054 ) ;
#6243 = CARTESIAN_POINT ( 'NONE',  ( -0.8893259633308450152, -1.753947465207011058, 2.849594321892158888 ) ) ;
#6244 = VERTEX_POINT ( 'NONE', #12694 ) ;
#6245 = CARTESIAN_POINT ( 'NONE',  ( 0.5500000000000000444, 6.450000000000000178, 3.600000000000000089 ) ) ;
#6246 = CARTESIAN_POINT ( 'NONE',  ( 1.722095088963199405, -0.7763906680874423927, 2.675734922583239861 ) ) ;
#6247 = CARTESIAN_POINT ( 'NONE',  ( -0.2041457401073759059, -1.101875393134940984, 7.346023093209487875 ) ) ;
#6248 = EDGE_LOOP ( 'NONE', ( #13273, #15977, #13076, #225 ) ) ;
#6249 = DIRECTION ( 'NONE',  ( 1.000000000000000000, 0.000000000000000000, 0.000000000000000000 ) ) ;
#6250 = CARTESIAN_POINT ( 'NONE',  ( 1.750000000000000000, 0.5999999999999999778, 7.599999999999999645 ) ) ;
#6251 = DIRECTION ( 'NONE',  ( 1.445602896647339508E-15, -1.000000000000000000, -1.264902534566422168E-15 ) ) ;
#6252 = CARTESIAN_POINT ( 'NONE',  ( -1.596341326794979976, -5.264406779661020330, 2.970780074643819990 ) ) ;
#6253 = ORIENTED_EDGE ( 'NONE', *, *, #6642, .F. ) ;
#6254 = ORIENTED_EDGE ( 'NONE', *, *, #2230, .F. ) ;
#6255 = LINE ( 'NONE', #11725, #15993 ) ;
#6256 = DIRECTION ( 'NONE',  ( 1.000000000000000000, -2.220446049250309876E-16, -6.123233995736769734E-17 ) ) ;
#6257 = CARTESIAN_POINT ( 'NONE',  ( 0.2254033459420760055, -0.6247245358507570456, 2.348900562125120217 ) ) ;
#6258 = ORIENTED_EDGE ( 'NONE', *, *, #16171, .T. ) ;
#6259 = CARTESIAN_POINT ( 'NONE',  ( -0.9490039995899379743, -2.076142624883081211, 2.221592224478750488 ) ) ;
#6260 = LINE ( 'NONE', #10805, #829 ) ;
#6261 = CARTESIAN_POINT ( 'NONE',  ( -1.000000000000000000, -6.000000000000000000, 3.673738709727309981 ) ) ;
#6262 = CARTESIAN_POINT ( 'NONE',  ( 0.6343239990445400656, -3.500569086828630105, 2.433641963034069988 ) ) ;
#6263 = AXIS2_PLACEMENT_3D ( 'NONE', #6772, #16674, #16492 ) ;
#6264 = CARTESIAN_POINT ( 'NONE',  ( 0.4944444514933294954, -5.311531839079339790, 2.693008931300498787 ) ) ;
#6265 = EDGE_CURVE ( 'NONE', #12426, #16167, #368, .T. ) ;
#6266 = CARTESIAN_POINT ( 'NONE',  ( -2.639965200365840037, -1.750106588847040845, 4.971472712918284742 ) ) ;
#6267 = DIRECTION ( 'NONE',  ( -1.000000000000000000, 0.000000000000000000, 0.000000000000000000 ) ) ;
#6268 = CARTESIAN_POINT ( 'NONE',  ( -2.350067830300900162, -0.5224576271186440746, 4.825253242917699303 ) ) ;
#6269 = DIRECTION ( 'NONE',  ( 1.000000000000000000, -1.903239470785979823E-16, 0.000000000000000000 ) ) ;
#6270 = CARTESIAN_POINT ( 'NONE',  ( -0.6500000000000000222, 6.450000000000000178, 2.699264068711930253 ) ) ;
#6271 = DIRECTION ( 'NONE',  ( 6.123233995736769734E-17, 2.493473113004670213E-16, 1.000000000000000000 ) ) ;
#6272 = CARTESIAN_POINT ( 'NONE',  ( -1.978267656359410154, -5.497669491525420504, 5.974740860598790171 ) ) ;
#6273 = ORIENTED_EDGE ( 'NONE', *, *, #17600, .F. ) ;
#6274 = DIRECTION ( 'NONE',  ( 1.908195823574489776E-16, -1.000000000000000000, -6.938893903907229610E-17 ) ) ;
#6275 = VERTEX_POINT ( 'NONE', #17276 ) ;
#6276 = DIRECTION ( 'NONE',  ( 0.000000000000000000, -1.000000000000000000, 0.000000000000000000 ) ) ;
#6277 = DIRECTION ( 'NONE',  ( 1.807003620809174583E-15, 1.000000000000000000, 1.807003620809174385E-16 ) ) ;
#6278 = ORIENTED_EDGE ( 'NONE', *, *, #7598, .F. ) ;
#6279 = VECTOR ( 'NONE', #10208, 1000.000000000000000 ) ;
#6280 = CARTESIAN_POINT ( 'NONE',  ( 1.167621112247380077, -2.821367850108300157, 6.743381174846749815 ) ) ;
#6281 = CARTESIAN_POINT ( 'NONE',  ( 1.943632316591230147, -5.346398305084740343, 3.373048379518159834 ) ) ;
#6282 = CARTESIAN_POINT ( 'NONE',  ( 0.000000000000000000, -5.599999999999999645, -3.429011037612589769E-16 ) ) ;
#6283 = CARTESIAN_POINT ( 'NONE',  ( -2.308170020371289599, -1.726818300558750074, 5.159452766389659217 ) ) ;
#6284 = CARTESIAN_POINT ( 'NONE',  ( -1.917298190932639868, -3.496728210468659892, 3.335187436117939885 ) ) ;
#6285 = CARTESIAN_POINT ( 'NONE',  ( 2.032257487115179728, -1.028169651910100679, 4.991258216523873692 ) ) ;
#6286 = ADVANCED_FACE ( 'NONE', ( #4338 ), #15922, .T. ) ;
#6287 = CYLINDRICAL_SURFACE ( 'NONE', #13233, 0.2500000000000002220 ) ;
#6288 = DIRECTION ( 'NONE',  ( 1.189524669241239855E-16, -1.000000000000000000, 0.000000000000000000 ) ) ;
#6289 = ORIENTED_EDGE ( 'NONE', *, *, #758, .T. ) ;
#6290 = EDGE_CURVE ( 'NONE', #12675, #4902, #10096, .T. ) ;
#6291 = DIRECTION ( 'NONE',  ( -1.000000000000000000, 1.776356839399180454E-14, 0.000000000000000000 ) ) ;
#6292 = CARTESIAN_POINT ( 'NONE',  ( 1.392553072310509510, -0.3355932203389832558, 3.191531554476519261 ) ) ;
#6293 = CARTESIAN_POINT ( 'NONE',  ( 2.353452300571019506, -4.125511994252439862, 4.697179287168359529 ) ) ;
#6294 = VERTEX_POINT ( 'NONE', #1847 ) ;
#6295 = ADVANCED_FACE ( 'NONE', ( #14609 ), #14799, .F. ) ;
#6296 = VERTEX_POINT ( 'NONE', #7761 ) ;
#6297 = EDGE_CURVE ( 'NONE', #12628, #2833, #4510, .T. ) ;
#6298 = DIRECTION ( 'NONE',  ( 0.000000000000000000, 0.000000000000000000, 1.000000000000000000 ) ) ;
#6299 = EDGE_LOOP ( 'NONE', ( #15209, #12122, #12133, #12620 ) ) ;
#6300 = CARTESIAN_POINT ( 'NONE',  ( -2.151546283159489814, -4.711560077819619607, 3.746273477677510844 ) ) ;
#6301 = CARTESIAN_POINT ( 'NONE',  ( 0.2812789908084389889, -5.144279661016950556, 7.036533610117280624 ) ) ;
#6302 = VECTOR ( 'NONE', #13292, 1000.000000000000000 ) ;
#6303 = DIRECTION ( 'NONE',  ( -1.000000000000000000, 0.000000000000000000, 7.273661547324610053E-16 ) ) ;
#6304 = CARTESIAN_POINT ( 'NONE',  ( 2.345900685764729765, -0.3711864406779670222, 4.512231114381330066 ) ) ;
#6305 = ORIENTED_EDGE ( 'NONE', *, *, #2237, .T. ) ;
#6306 = PLANE ( 'NONE',  #14123 ) ;
#6307 = CARTESIAN_POINT ( 'NONE',  ( -0.03076623656502111559, -4.521412895153344103, 6.752792069673816400 ) ) ;
#6308 = CARTESIAN_POINT ( 'NONE',  ( -2.625437065641401446, -0.5180084745762725262, 5.087214675345155257 ) ) ;
#6309 = EDGE_LOOP ( 'NONE', ( #666, #10664, #4581, #11281 ) ) ;
#6310 = CARTESIAN_POINT ( 'NONE',  ( -1.782460458101500889, -0.5002118644067795605, 5.718585207845990226 ) ) ;
#6311 = EDGE_CURVE ( 'NONE', #3727, #12747, #13528, .T. ) ;
#6312 = CARTESIAN_POINT ( 'NONE',  ( 1.347262683220810553, -0.4245762711864407013, 6.986424775243341045 ) ) ;
#6313 = VERTEX_POINT ( 'NONE', #10749 ) ;
#6314 = CARTESIAN_POINT ( 'NONE',  ( -2.011500846714319835, -5.551059322033900401, 3.478373409938470218 ) ) ;
#6315 = DIRECTION ( 'NONE',  ( 1.000000000000000000, -1.480297366166879989E-15, 0.000000000000000000 ) ) ;
#6316 = CARTESIAN_POINT ( 'NONE',  ( -0.8242394280876598200, -1.171740257999809964, 6.904399023015030501 ) ) ;
#6317 = CARTESIAN_POINT ( 'NONE',  ( -1.061361729696689515, -0.2742238837839081067, 2.926312958971010847 ) ) ;
#6318 = CARTESIAN_POINT ( 'NONE',  ( -2.008025181017680794, -3.520016498756949552, 2.964791492240541171 ) ) ;
#6319 = VERTEX_POINT ( 'NONE', #11951 ) ;
#6320 = CARTESIAN_POINT ( 'NONE',  ( -2.322440385110939864, -3.081379897639439758, 4.319189883157439347 ) ) ;
#6321 = CARTESIAN_POINT ( 'NONE',  ( 1.750000000000000000, 0.5999999999999999778, 7.599999999999999645 ) ) ;
#6322 = CARTESIAN_POINT ( 'NONE',  ( -8.878689293818318209E-17, 6.750000000000000000, 5.100000000000000533 ) ) ;
#6323 = CARTESIAN_POINT ( 'NONE',  ( 2.041954431566909367, -3.849893411152959910, 4.912894203848615859 ) ) ;
#6324 = DIRECTION ( 'NONE',  ( -1.306144734853129823E-16, 1.000000000000000000, 0.000000000000000000 ) ) ;
#6325 = DIRECTION ( 'NONE',  ( 0.000000000000000000, -1.000000000000000000, -1.359631073446889961E-32 ) ) ;
#6326 = CARTESIAN_POINT ( 'NONE',  ( -1.736825397686170502, -1.614217735477279536, 3.605313112995154334 ) ) ;
#6327 = ORIENTED_EDGE ( 'NONE', *, *, #1673, .T. ) ;
#6328 = FACE_OUTER_BOUND ( 'NONE', #2095, .T. ) ;
#6329 = EDGE_CURVE ( 'NONE', #12197, #16406, #13008, .T. ) ;
#6330 = FACE_OUTER_BOUND ( 'NONE', #9462, .T. ) ;
#6331 = ORIENTED_EDGE ( 'NONE', *, *, #11407, .F. ) ;
#6332 = DIRECTION ( 'NONE',  ( 0.000000000000000000, 1.306144734853129823E-16, -1.000000000000000000 ) ) ;
#6333 = LINE ( 'NONE', #1321, #8681 ) ;
#6334 = FACE_OUTER_BOUND ( 'NONE', #17770, .T. ) ;
#6335 = CARTESIAN_POINT ( 'NONE',  ( -2.353194804772640314, -5.224364406779660186, 4.731327187377240229 ) ) ;
#6336 = ORIENTED_EDGE ( 'NONE', *, *, #17482, .T. ) ;
#6337 = ORIENTED_EDGE ( 'NONE', *, *, #11074, .F. ) ;
#6338 = CARTESIAN_POINT ( 'NONE',  ( -1.899999999999999911, 4.700000000000000178, 1.600000000000000089 ) ) ;
#6339 = CARTESIAN_POINT ( 'NONE',  ( -1.250000000000000000, 7.799999999999999822, 7.599999999999999645 ) ) ;
#6340 = DIRECTION ( 'NONE',  ( 1.000000000000000000, -2.220446049250309876E-16, -7.273661547324610053E-16 ) ) ;
#6341 = ORIENTED_EDGE ( 'NONE', *, *, #5630, .T. ) ;
#6342 = CARTESIAN_POINT ( 'NONE',  ( -1.965557623688110933, -5.511016949152534927, 5.292675575926340414 ) ) ;
#6343 = CARTESIAN_POINT ( 'NONE',  ( 2.574214976178930137, -2.196424942684489956, 4.054607910322744146 ) ) ;
#6344 = DIRECTION ( 'NONE',  ( -6.123233995736769734E-17, 2.611996170812411923E-32, -1.000000000000000000 ) ) ;
#6345 = CARTESIAN_POINT ( 'NONE',  ( -1.071153154657450202, -3.054250732991181216, 7.128115444592631356 ) ) ;
#6346 = CARTESIAN_POINT ( 'NONE',  ( 1.000000000000002220, 9.099999999999999645, 7.700000000000000178 ) ) ;
#6347 = LINE ( 'NONE', #17912, #7046 ) ;
#6348 = CARTESIAN_POINT ( 'NONE',  ( -1.611907055891630192, -3.244397915657459830, 2.985210995296889713 ) ) ;
#6349 = CARTESIAN_POINT ( 'NONE',  ( -1.550000000000000044, -5.599999999999999645, 5.100000000000000533 ) ) ;
#6350 = DIRECTION ( 'NONE',  ( 0.000000000000000000, 0.000000000000000000, 1.000000000000000000 ) ) ;
#6352 = EDGE_LOOP ( 'NONE', ( #11305, #15885, #14830, #16309, #2217, #12421, #14481, #16002, #15049, #272, #10586, #8373, #15420, #5565 ) ) ;
#6351 = CARTESIAN_POINT ( 'NONE',  ( 1.901407128523888934, -2.751502985243430288, 6.551422324754781812 ) ) ;
#6353 = EDGE_CURVE ( 'NONE', #3882, #6244, #16305, .T. ) ;
#6354 = LINE ( 'NONE', #12019, #2328 ) ;
#6355 = DIRECTION ( 'NONE',  ( 0.000000000000000000, 0.000000000000000000, 1.000000000000000000 ) ) ;
#6356 = CARTESIAN_POINT ( 'NONE',  ( -2.091095264232510242, -1.656953435693890198, 5.779845490516250628 ) ) ;
#6357 = LINE ( 'NONE', #16285, #17131 ) ;
#6358 = CARTESIAN_POINT ( 'NONE',  ( -2.088297318559229954, -5.502118644067800268, 5.785136623276639689 ) ) ;
#6359 = ORIENTED_EDGE ( 'NONE', *, *, #3604, .F. ) ;
#6360 = PRODUCT_DEFINITION_SHAPE ( 'NONE', 'NONE',  #18301 ) ;
#6361 = CARTESIAN_POINT ( 'NONE',  ( 0.2270348434643680025, -5.304612347394249916, 2.348896311281980065 ) ) ;
#6362 = ORIENTED_EDGE ( 'NONE', *, *, #15735, .F. ) ;
#6363 = LINE ( 'NONE', #2021, #1386 ) ;
#6364 = DIRECTION ( 'NONE',  ( -0.000000000000000000, 1.000000000000000000, 0.000000000000000000 ) ) ;
#6365 = ORIENTED_EDGE ( 'NONE', *, *, #7277, .T. ) ;
#6366 = ORIENTED_EDGE ( 'NONE', *, *, #12580, .T. ) ;
#6367 = CARTESIAN_POINT ( 'NONE',  ( 0.1226612266411070129, -2.937809291549740021, 7.050255286338659388 ) ) ;
#6368 = FACE_OUTER_BOUND ( 'NONE', #3644, .T. ) ;
#6369 = CARTESIAN_POINT ( 'NONE',  ( -1.596341326794979976, -5.564406779661021041, 2.970780074643819990 ) ) ;
#6370 = CARTESIAN_POINT ( 'NONE',  ( 1.850000000000000089, -5.599999999999999645, 2.299999999999999822 ) ) ;
#6371 = AXIS2_PLACEMENT_3D ( 'NONE', #5454, #2583, #12307 ) ;
#6372 = CARTESIAN_POINT ( 'NONE',  ( 1.902324933209389890, -2.402178660919109809, 3.314393441133530072 ) ) ;
#6373 = CARTESIAN_POINT ( 'NONE',  ( -0.8986180677147959095, -3.636457940198390304, 2.524860635301629852 ) ) ;
#6374 = CARTESIAN_POINT ( 'NONE',  ( 0.2475374578675958726, -1.354205687946139491, 6.738044908627027318 ) ) ;
#6375 = VECTOR ( 'NONE', #7844, 1000.000000000000000 ) ;
#6376 = CARTESIAN_POINT ( 'NONE',  ( -6.735557395310420329E-17, 6.700000000000000178, 6.299999999999999822 ) ) ;
#6377 = CARTESIAN_POINT ( 'NONE',  ( -2.500000000000000000, 11.29999999999999893, 7.649999999999999467 ) ) ;
#6378 = VERTEX_POINT ( 'NONE', #2139 ) ;
#6379 = DIRECTION ( 'NONE',  ( -2.018587317500279868E-16, 1.000000000000000000, 5.046468293750709530E-17 ) ) ;
#6380 = CARTESIAN_POINT ( 'NONE',  ( -0.6918414964982418924, -3.659746228486680408, 2.450533167346770291 ) ) ;
#6381 = ORIENTED_EDGE ( 'NONE', *, *, #2479, .F. ) ;
#6382 = ORIENTED_EDGE ( 'NONE', *, *, #10319, .T. ) ;
#6383 = LINE ( 'NONE', #658, #5280 ) ;
#6384 = ORIENTED_EDGE ( 'NONE', *, *, #5971, .T. ) ;
#6385 = CARTESIAN_POINT ( 'NONE',  ( 0.1749999999999999889, 9.500000000000000000, 3.100000000000000089 ) ) ;
#6386 = CONTEXT_DEPENDENT_SHAPE_REPRESENTATION ( #3647, #3877 ) ;
#6387 = CARTESIAN_POINT ( 'NONE',  ( 1.112838723655040107, -5.126483050847459921, 6.773667561836210105 ) ) ;
#6388 = CYLINDRICAL_SURFACE ( 'NONE', #17631, 0.9499999999999999556 ) ;
#6389 = EDGE_LOOP ( 'NONE', ( #15372, #2142, #8196, #1003 ) ) ;
#6390 = EDGE_CURVE ( 'NONE', #6904, #1389, #5191, .T. ) ;
#6391 = CARTESIAN_POINT ( 'NONE',  ( -0.2749999999999995781, 2.299999999999999822, 7.599999999999999645 ) ) ;
#6392 = EDGE_CURVE ( 'NONE', #16382, #6586, #11607, .T. ) ;
#6393 = CARTESIAN_POINT ( 'NONE',  ( -1.555285212483289659, -3.520016498756949552, 3.359854578615099285 ) ) ;
#6394 = AXIS2_PLACEMENT_3D ( 'NONE', #12196, #6440, #5058 ) ;
#6395 = CARTESIAN_POINT ( 'NONE',  ( -2.171642826483958899, -0.4957627118644069575, 6.225392547715731695 ) ) ;
#6396 = ORIENTED_EDGE ( 'NONE', *, *, #15381, .F. ) ;
#6397 = CARTESIAN_POINT ( 'NONE',  ( 0.5500000000000000444, -2.399999999999999911, 3.600000000000000089 ) ) ;
#6398 = AXIS2_PLACEMENT_3D ( 'NONE', #1462, #4311, #14233 ) ;
#6399 = CARTESIAN_POINT ( 'NONE',  ( 2.458531667407859889, -0.09343220338983100615, 5.699238225248945966 ) ) ;
#6400 = AXIS2_PLACEMENT_3D ( 'NONE', #11664, #7502, #1936 ) ;
#6401 = ORIENTED_EDGE ( 'NONE', *, *, #11854, .F. ) ;
#6402 = FACE_OUTER_BOUND ( 'NONE', #15158, .T. ) ;
#6403 = CARTESIAN_POINT ( 'NONE',  ( 0.2564439965879029004, -1.055298816558370323, 7.039440566481206751 ) ) ;
#6404 = CARTESIAN_POINT ( 'NONE',  ( 2.155845792290829621, -5.355296610169490101, 3.756158857535770057 ) ) ;
#6405 = VECTOR ( 'NONE', #2623, 1000.000000000000000 ) ;
#6406 = CARTESIAN_POINT ( 'NONE',  ( 2.649108131072720695, -0.7059744922340407403, 4.859184807329644862 ) ) ;
#6407 = ORIENTED_EDGE ( 'NONE', *, *, #9830, .F. ) ;
#6408 = ADVANCED_FACE ( 'NONE', ( #2231 ), #744, .F. ) ;
#6409 = CARTESIAN_POINT ( 'NONE',  ( -0.5921572875253819923, 6.450000000000000178, 1.600000000000000089 ) ) ;
#6410 = CARTESIAN_POINT ( 'NONE',  ( 0.9485663501270550357, -2.545749267008810435, 6.853826262002240988 ) ) ;
#6411 = CARTESIAN_POINT ( 'NONE',  ( 2.550815101416278541, -4.195376859117311064, 5.432431574543660879 ) ) ;
#6412 = EDGE_CURVE ( 'NONE', #1792, #14614, #9064, .T. ) ;
#6413 = VECTOR ( 'NONE', #17796, 1000.000000000000000 ) ;
#6414 = LINE ( 'NONE', #17598, #10239 ) ;
#6415 = VECTOR ( 'NONE', #9315, 1000.000000000000000 ) ;
#6416 = DIRECTION ( 'NONE',  ( 5.103860808646520231E-18, -6.123233995736769734E-17, -1.000000000000000000 ) ) ;
#6417 = EDGE_CURVE ( 'NONE', #11376, #12725, #17237, .T. ) ;
#6418 = CARTESIAN_POINT ( 'NONE',  ( -2.025702773739959106, -3.081379897639443310, 4.366188503657674858 ) ) ;
#6419 = PLANE ( 'NONE',  #15009 ) ;
#6420 = CYLINDRICAL_SURFACE ( 'NONE', #2645, 0.2000000000000000944 ) ;
#6421 = CARTESIAN_POINT ( 'NONE',  ( 0.03076623656506880661, -1.078587104846650213, 6.752792069673816400 ) ) ;
#6422 = EDGE_LOOP ( 'NONE', ( #6131, #4771, #7735, #13474 ) ) ;
#6423 = FACE_OUTER_BOUND ( 'NONE', #7467, .T. ) ;
#6424 = AXIS2_PLACEMENT_3D ( 'NONE', #15739, #12948, #12858 ) ;
#6425 = VECTOR ( 'NONE', #719, 1000.000000000000000 ) ;
#6426 = CARTESIAN_POINT ( 'NONE',  ( 0.2151249875495270247, -0.3251990024832489556, 2.650810719223910983 ) ) ;
#6427 = CARTESIAN_POINT ( 'NONE',  ( -2.146130664537640786, -3.197821339080880065, 3.138834773724098692 ) ) ;
#6428 = VERTEX_POINT ( 'NONE', #7783 ) ;
#6429 = FACE_OUTER_BOUND ( 'NONE', #748, .T. ) ;
#6430 = CARTESIAN_POINT ( 'NONE',  ( 0.06276132972186961034, -1.377493976234430040, 7.052616990284530374 ) ) ;
#6431 = DIRECTION ( 'NONE',  ( 0.000000000000000000, 0.000000000000000000, 1.000000000000000000 ) ) ;
#6432 = CARTESIAN_POINT ( 'NONE',  ( -2.088297318559229954, -5.202118644067800446, 5.785136623276639689 ) ) ;
#6433 = ORIENTED_EDGE ( 'NONE', *, *, #6137, .F. ) ;
#6434 = AXIS2_PLACEMENT_3D ( 'NONE', #16630, #5507, #15343 ) ;
#6435 = EDGE_CURVE ( 'NONE', #11001, #14847, #336, .T. ) ;
#6436 = VECTOR ( 'NONE', #10501, 1000.000000000000000 ) ;
#6437 = EDGE_LOOP ( 'NONE', ( #10207, #15695, #11755, #5049 ) ) ;
#6438 = FACE_OUTER_BOUND ( 'NONE', #11881, .T. ) ;
#6439 = DIRECTION ( 'NONE',  ( 0.000000000000000000, 0.000000000000000000, 1.000000000000000000 ) ) ;
#6440 = DIRECTION ( 'NONE',  ( 0.000000000000000000, 0.000000000000000000, 1.000000000000000000 ) ) ;
#6441 = ORIENTED_EDGE ( 'NONE', *, *, #9347, .F. ) ;
#6442 = CARTESIAN_POINT ( 'NONE',  ( -0.7476103186298618253, -5.582203389830510787, 2.787995836256459636 ) ) ;
#6443 = VECTOR ( 'NONE', #10949, 1000.000000000000000 ) ;
#6444 = AXIS2_PLACEMENT_3D ( 'NONE', #12131, #16105, #11851 ) ;
#6445 = CARTESIAN_POINT ( 'NONE',  ( -2.594645788401189090, -2.988226744486289999, 5.257608218854294968 ) ) ;
#6446 = DIRECTION ( 'NONE',  ( 1.059690869644410208E-14, 1.000000000000000000, -1.041146930477340028E-32 ) ) ;
#6447 = CARTESIAN_POINT ( 'NONE',  ( 2.065789008933020199, -2.728214696955149510, 6.366022047745297563 ) ) ;
#6448 = EDGE_CURVE ( 'NONE', #5712, #1195, #1369, .T. ) ;
#6449 = DIRECTION ( 'NONE',  ( 1.000000000000000000, 0.000000000000000000, 0.000000000000000000 ) ) ;
#6450 = CARTESIAN_POINT ( 'NONE',  ( -2.500000000000000000, 4.700000000000000178, 1.600000000000000089 ) ) ;
#6451 = CARTESIAN_POINT ( 'NONE',  ( -1.644832646965619816, -4.408812330071869567, 6.383232381746489992 ) ) ;
#6452 = CARTESIAN_POINT ( 'NONE',  ( 1.661700935788380074, -5.337500000000000355, 3.038299064211610112 ) ) ;
#6453 = AXIS2_PLACEMENT_3D ( 'NONE', #13362, #4748, #13274 ) ;
#6454 = PLANE ( 'NONE',  #16230 ) ;
#6456 = VERTEX_POINT ( 'NONE', #5641 ) ;
#6455 = CARTESIAN_POINT ( 'NONE',  ( -1.788074174585561060, -1.982989471729918352, 2.738902236199820539 ) ) ;
#6457 = PLANE ( 'NONE',  #7615 ) ;
#6458 = DIRECTION ( 'NONE',  ( 0.000000000000000000, 0.000000000000000000, 1.000000000000000000 ) ) ;
#6459 = CARTESIAN_POINT ( 'NONE',  ( 1.057242234132090175, -0.3222457627118650025, 2.597442975781520058 ) ) ;
#6460 = VECTOR ( 'NONE', #7583, 1000.000000000000000 ) ;
#6461 = CARTESIAN_POINT ( 'NONE',  ( 1.265407828724300021, -2.309025507765960050, 2.715689360385540319 ) ) ;
#6462 = CARTESIAN_POINT ( 'NONE',  ( -0.009452110982656868748, -5.299807955295460005, 2.350000000000000089 ) ) ;
#6463 = VECTOR ( 'NONE', #11319, 1000.000000000000000 ) ;
#6464 = CARTESIAN_POINT ( 'NONE',  ( 0.9000000000000000222, 2.050000000000000266, 3.600000000000000089 ) ) ;
#6465 = CARTESIAN_POINT ( 'NONE',  ( -2.180207327701300102, -5.506567796610169374, 5.586116916730199833 ) ) ;
#6466 = ORIENTED_EDGE ( 'NONE', *, *, #13199, .F. ) ;
#6467 = EDGE_CURVE ( 'NONE', #11652, #15772, #11438, .T. ) ;
#6468 = CARTESIAN_POINT ( 'NONE',  ( -1.889999999999999902, 4.100000000000000533, -6.851683986394989688E-16 ) ) ;
#6469 = ORIENTED_EDGE ( 'NONE', *, *, #129, .F. ) ;
#6470 = DIRECTION ( 'NONE',  ( 0.2721173643531200059, -0.9622640697945191723, 0.000000000000000000 ) ) ;
#6471 = DIRECTION ( 'NONE',  ( 0.000000000000000000, 0.000000000000000000, -1.000000000000000000 ) ) ;
#6472 = VERTEX_POINT ( 'NONE', #17009 ) ;
#6473 = ADVANCED_FACE ( 'NONE', ( #10158 ), #7295, .T. ) ;
#6474 = ORIENTED_EDGE ( 'NONE', *, *, #6563, .T. ) ;
#6475 = CARTESIAN_POINT ( 'NONE',  ( 2.126557263589630153, -2.448755237495689574, 3.691783806836010040 ) ) ;
#6476 = EDGE_CURVE ( 'NONE', #8985, #11075, #2962, .T. ) ;
#6477 = CARTESIAN_POINT ( 'NONE',  ( -2.011500846714319835, -5.551059322033900401, 3.478373409938470218 ) ) ;
#6478 = VECTOR ( 'NONE', #1001, 1000.000000000000000 ) ;
#6479 = DIRECTION ( 'NONE',  ( 2.220446049250309876E-16, 0.000000000000000000, -1.000000000000000000 ) ) ;
#6480 = CARTESIAN_POINT ( 'NONE',  ( 1.832842064134690085, -2.728214696955149954, 6.176291182464479945 ) ) ;
#6481 = LINE ( 'NONE', #12140, #770 ) ;
#6482 = CARTESIAN_POINT ( 'NONE',  ( -1.043047520545169471, -1.517223705964159786, 6.468319459971155538 ) ) ;
#6483 = CARTESIAN_POINT ( 'NONE',  ( 2.616666666666660035, 8.899094389694600942E-17, 4.000000000000000000 ) ) ;
#6484 = LINE ( 'NONE', #5290, #5314 ) ;
#6485 = ORIENTED_EDGE ( 'NONE', *, *, #15636, .T. ) ;
#6486 = CARTESIAN_POINT ( 'NONE',  ( 1.568166175152220010, -0.5822263355386709804, 3.139533976446129859 ) ) ;
#6487 = DIRECTION ( 'NONE',  ( -1.000000000000000000, -1.850371707708589879E-16, 0.000000000000000000 ) ) ;
#6488 = CARTESIAN_POINT ( 'NONE',  ( 2.313035575219750228, -4.172088570829020071, 5.134294963419709923 ) ) ;
#6489 = ORIENTED_EDGE ( 'NONE', *, *, #18289, .F. ) ;
#6490 = VECTOR ( 'NONE', #17213, 1000.000000000000000 ) ;
#6491 = VERTEX_POINT ( 'NONE', #7135 ) ;
#6492 = CARTESIAN_POINT ( 'NONE',  ( -1.899999999999999911, 2.000000000000000000, 2.388061258337340122E-16 ) ) ;
#6493 = EDGE_LOOP ( 'NONE', ( #10469, #2613, #345, #4864 ) ) ;
#6494 = LINE ( 'NONE', #17772, #16599 ) ;
#6495 = EDGE_CURVE ( 'NONE', #15295, #13116, #9895, .T. ) ;
#6496 = SHAPE_DEFINITION_REPRESENTATION ( #10670, #4614 ) ;
#6497 = CARTESIAN_POINT ( 'NONE',  ( 1.300961508564179914, -5.122033898305089927, 6.661123742937279602 ) ) ;
#6498 = FACE_OUTER_BOUND ( 'NONE', #330, .T. ) ;
#6499 = EDGE_LOOP ( 'NONE', ( #5718, #7029, #16325, #4903, #7440, #8677, #9151, #17926, #7531, #5618, #3524, #3418, #6946, #12329, #16991, #14478 ) ) ;
#6500 = CARTESIAN_POINT ( 'NONE',  ( -2.262450597846770162, -1.404623140882689913, 5.348122657979730299 ) ) ;
#6501 = CARTESIAN_POINT ( 'NONE',  ( 1.000000000000000000, 5.400000000000000355, 8.300000000000000711 ) ) ;
#6502 = AXIS2_PLACEMENT_3D ( 'NONE', #12671, #13876, #11456 ) ;
#6503 = CARTESIAN_POINT ( 'NONE',  ( 0.8967027089123184025, -4.404971453711897134, 6.546842195331636916 ) ) ;
#6504 = EDGE_CURVE ( 'NONE', #7625, #10238, #8679, .T. ) ;
#6505 = CARTESIAN_POINT ( 'NONE',  ( 0.7983658734558030101, -0.1334745762711870010, 6.913847129767330735 ) ) ;
#6506 = ORIENTED_EDGE ( 'NONE', *, *, #11612, .T. ) ;
#6507 = CARTESIAN_POINT ( 'NONE',  ( -2.651721837666119796, -0.2269067796610169385, 4.594045830208265180 ) ) ;
#6508 = ORIENTED_EDGE ( 'NONE', *, *, #782, .F. ) ;
#6509 = CARTESIAN_POINT ( 'NONE',  ( -1.750316316486840051, -5.559957627118639500, 3.126818518378589928 ) ) ;
#6510 = CARTESIAN_POINT ( 'NONE',  ( -1.728413393879669968, -1.288181699441249606, 6.297289212178331042 ) ) ;
#6511 = ADVANCED_FACE ( 'NONE', ( #16837 ), #4423, .F. ) ;
#6512 = AXIS2_PLACEMENT_3D ( 'NONE', #15530, #2831, #8478 ) ;
#6513 = CARTESIAN_POINT ( 'NONE',  ( 0.4974685680287860290, -5.439830508474580384, 7.000224381598740386 ) ) ;
#6514 = CARTESIAN_POINT ( 'NONE',  ( -2.649108131072720695, -4.894025507765944916, 4.859184807329705258 ) ) ;
#6515 = EDGE_LOOP ( 'NONE', ( #12253, #13717, #12617, #14585 ) ) ;
#6516 = DIRECTION ( 'NONE',  ( -3.700743415417180054E-15, -1.000000000000000000, -1.850371707708589879E-16 ) ) ;
#6517 = CARTESIAN_POINT ( 'NONE',  ( 2.345213174852950111, -3.803316834576380145, 4.503223853122319653 ) ) ;
#6518 = CARTESIAN_POINT ( 'NONE',  ( -0.5500000000000000444, 7.799999999999999822, 1.600000000000000089 ) ) ;
#6519 = CARTESIAN_POINT ( 'NONE',  ( -1.899999999999999911, 2.000000000000000000, 1.600000000000000089 ) ) ;
#6520 = CARTESIAN_POINT ( 'NONE',  ( -0.3943683997330095781, -3.384127645387192018, 2.685210827922659860 ) ) ;
#6521 = DIRECTION ( 'NONE',  ( -1.000000000000000000, -3.700743415417190112E-16, -3.700743415417190112E-16 ) ) ;
#6522 = CARTESIAN_POINT ( 'NONE',  ( -2.500000000000000000, 1.071484571201660082E-16, 3.600000000000000089 ) ) ;
#6523 = ADVANCED_FACE ( 'NONE', ( #15554 ), #16925, .T. ) ;
#6524 = CARTESIAN_POINT ( 'NONE',  ( -0.3429245540020551819, -1.823812330071880705, 2.675820019639910452 ) ) ;
#6525 = EDGE_LOOP ( 'NONE', ( #15621, #5598, #13381, #9679 ) ) ;
#6526 = CARTESIAN_POINT ( 'NONE',  ( 0.5000000000000000000, 4.631370849898480024, 5.100000000000000533 ) ) ;
#6527 = EDGE_CURVE ( 'NONE', #1744, #13435, #7210, .T. ) ;
#6528 = AXIS2_PLACEMENT_3D ( 'NONE', #16923, #11093, #2960 ) ;
#6529 = DIRECTION ( 'NONE',  ( 1.000000000000000000, 3.172065784643300034E-16, 2.220446049250309876E-16 ) ) ;
#6530 = EDGE_CURVE ( 'NONE', #17179, #7642, #12372, .T. ) ;
#6531 = CARTESIAN_POINT ( 'NONE',  ( 1.864786684738361178, -0.7952867690272208412, 2.817120744449660652 ) ) ;
#6532 = CARTESIAN_POINT ( 'NONE',  ( 2.502804106625939440, -2.173136654396201184, 3.817341913956370458 ) ) ;
#6533 = VERTEX_POINT ( 'NONE', #8506 ) ;
#6534 = CARTESIAN_POINT ( 'NONE',  ( -1.229686204202100175, -5.164643153926309793, 2.674737924334550154 ) ) ;
#6535 = CARTESIAN_POINT ( 'NONE',  ( 1.869504824896970119, -5.095338983050850423, 5.548311746956850143 ) ) ;
#6536 = ORIENTED_EDGE ( 'NONE', *, *, #758, .F. ) ;
#6537 = EDGE_CURVE ( 'NONE', #2694, #8350, #12770, .T. ) ;
#6538 = ORIENTED_EDGE ( 'NONE', *, *, #1464, .F. ) ;
#6539 = DIRECTION ( 'NONE',  ( -1.000000000000000000, 0.000000000000000000, -2.400482215405740060E-16 ) ) ;
#6540 = EDGE_CURVE ( 'NONE', #12255, #5832, #14156, .T. ) ;
#6541 = CARTESIAN_POINT ( 'NONE',  ( 2.500000000000000000, 2.799999999999999822, 1.600000000000000089 ) ) ;
#6542 = LINE ( 'NONE', #12108, #208 ) ;
#6543 = EDGE_CURVE ( 'NONE', #10849, #10826, #11375, .T. ) ;
#6544 = ORIENTED_EDGE ( 'NONE', *, *, #9976, .F. ) ;
#6545 = CARTESIAN_POINT ( 'NONE',  ( -0.7983658734557950165, -5.466525423728810118, 6.913847129767330735 ) ) ;
#6546 = CARTESIAN_POINT ( 'NONE',  ( 2.479511223993269287, -3.733451969711523155, 3.753882785753661633 ) ) ;
#6547 = CYLINDRICAL_SURFACE ( 'NONE', #14470, 0.04999999999999969746 ) ;
#6548 = CARTESIAN_POINT ( 'NONE',  ( -2.632194480419669080, -3.310421904162345719, 5.038623552414950524 ) ) ;
#6549 = DIRECTION ( 'NONE',  ( 1.000000000000000000, -1.059690869644410208E-14, 0.000000000000000000 ) ) ;
#6550 = DIRECTION ( 'NONE',  ( -8.269460797427580527E-16, 0.000000000000000000, 1.000000000000000000 ) ) ;
#6551 = CARTESIAN_POINT ( 'NONE',  ( -1.794646911016549939, -4.432100618360159672, 6.222494056560700315 ) ) ;
#6552 = CARTESIAN_POINT ( 'NONE',  ( -1.550000000000000044, -6.000000000000000000, 5.100000000000000533 ) ) ;
#6553 = CARTESIAN_POINT ( 'NONE',  ( -0.2335786437626909962, 6.450000000000000178, 1.958578643762689753 ) ) ;
#6555 = ORIENTED_EDGE ( 'NONE', *, *, #13500, .F. ) ;
#6554 = CARTESIAN_POINT ( 'NONE',  ( 1.991177874369370882, -2.378890372630820149, 2.945484578117438801 ) ) ;
#6556 = CARTESIAN_POINT ( 'NONE',  ( 1.899999999999999911, 8.500000000000000000, 0.6099999999999999867 ) ) ;
#6557 = LINE ( 'NONE', #2310, #10547 ) ;
#6558 = CARTESIAN_POINT ( 'NONE',  ( 0.4539185741479240255, -2.215872354612800521, 2.390735265170440105 ) ) ;
#6559 = CARTESIAN_POINT ( 'NONE',  ( 0.007090208766911279895, -5.037626194832210302, 2.248104425785700133 ) ) ;
#6560 = DIRECTION ( 'NONE',  ( 0.000000000000000000, -1.000000000000000000, 0.000000000000000000 ) ) ;
#6561 = CARTESIAN_POINT ( 'NONE',  ( -2.318251751302029984, -5.533262711864409766, 4.294764266798999586 ) ) ;
#6562 = ORIENTED_EDGE ( 'NONE', *, *, #13220, .F. ) ;
#6563 = EDGE_CURVE ( 'NONE', #7957, #7912, #9806, .T. ) ;
#6564 = CARTESIAN_POINT ( 'NONE',  ( 0.5999999999999999778, 11.40000000000000036, 7.700000000000000178 ) ) ;
#6565 = CARTESIAN_POINT ( 'NONE',  ( 2.351526912647309953, -5.073093220338978249, 4.606040641882800379 ) ) ;
#6566 = DIRECTION ( 'NONE',  ( -6.239269890455420182E-16, 5.872254014546280719E-16, -1.000000000000000000 ) ) ;
#6567 = CYLINDRICAL_SURFACE ( 'NONE', #6765, 0.6000000000000000888 ) ;
#6568 = VERTEX_POINT ( 'NONE', #15813 ) ;
#6569 = CARTESIAN_POINT ( 'NONE',  ( 1.991984774470479946, -3.985782264522710339, 3.446707398186009907 ) ) ;
#6570 = PLANE ( 'NONE',  #18247 ) ;
#6571 = CARTESIAN_POINT ( 'NONE',  ( -2.088297318559229954, -5.502118644067800268, 5.785136623276639689 ) ) ;
#6572 = DIRECTION ( 'NONE',  ( 6.123233995736769734E-17, 0.000000000000000000, 1.000000000000000000 ) ) ;
#6573 = CARTESIAN_POINT ( 'NONE',  ( -0.3159454637156809409, -2.984385868126319785, 7.032150113402090064 ) ) ;
#6574 = CARTESIAN_POINT ( 'NONE',  ( -1.820241257191459905, -5.080331814072259533, 3.208199930689799917 ) ) ;
#6575 = CARTESIAN_POINT ( 'NONE',  ( -0.3257255101953093757, -1.424070552811000701, 6.727018681373241549 ) ) ;
#6576 = FACE_OUTER_BOUND ( 'NONE', #10211, .T. ) ;
#6577 = CARTESIAN_POINT ( 'NONE',  ( -0.5500000000000000444, 2.050000000000000266, 3.600000000000000089 ) ) ;
#6578 = ORIENTED_EDGE ( 'NONE', *, *, #2845, .T. ) ;
#6579 = CARTESIAN_POINT ( 'NONE',  ( 1.595232607690389992, -5.306696984248650217, 3.104767392309609964 ) ) ;
#6580 = EDGE_CURVE ( 'NONE', #16962, #7679, #3041, .T. ) ;
#6581 = CARTESIAN_POINT ( 'NONE',  ( 1.250000000000000000, 3.500000000000000000, 5.100000000000000533 ) ) ;
#6582 = CARTESIAN_POINT ( 'NONE',  ( -1.092567884283820012, -4.637854336594780413, 6.784476218553590066 ) ) ;
#6583 = EDGE_LOOP ( 'NONE', ( #9958, #11679 ) ) ;
#6584 = VERTEX_POINT ( 'NONE', #5547 ) ;
#6585 = UNCERTAINTY_MEASURE_WITH_UNIT (LENGTH_MEASURE( 1.000000000000000082E-05 ), #12259, 'distance_accuracy_value', 'NONE');
#6586 = VERTEX_POINT ( 'NONE', #14054 ) ;
#6587 = CARTESIAN_POINT ( 'NONE',  ( 1.399999999999999911, 5.799999999999999822, 7.700000000000000178 ) ) ;
#6588 = CARTESIAN_POINT ( 'NONE',  ( -2.270487904532170198, -5.237711864406779938, 4.080813552109679776 ) ) ;
#6589 = DIRECTION ( 'NONE',  ( 1.445602896647339508E-15, 1.000000000000000000, 1.332267629550190412E-15 ) ) ;
#6590 = ORIENTED_EDGE ( 'NONE', *, *, #6705, .F. ) ;
#6591 = CARTESIAN_POINT ( 'NONE',  ( -2.629224451638860760, -4.641695212954759064, 4.339039509243916015 ) ) ;
#6592 = CARTESIAN_POINT ( 'NONE',  ( -1.000000000000000000, -5.000000000000000000, 6.100000000000000533 ) ) ;
#6593 = CARTESIAN_POINT ( 'NONE',  ( -2.345213174852959881, -1.796683165423619943, 4.503223853122380049 ) ) ;
#6594 = CARTESIAN_POINT ( 'NONE',  ( 1.000896394980339998, -0.1290254237288140093, 6.829956240957369751 ) ) ;
#6595 = VERTEX_POINT ( 'NONE', #7478 ) ;
#6596 = CARTESIAN_POINT ( 'NONE',  ( 2.203023580853990193, -0.3578389830508479919, 3.872235369154280349 ) ) ;
#6597 = CARTESIAN_POINT ( 'NONE',  ( 0.2189795514005130062, -0.3044491525423729805, 2.356806637999009801 ) ) ;
#6598 = ORIENTED_EDGE ( 'NONE', *, *, #12778, .F. ) ;
#6599 = ORIENTED_EDGE ( 'NONE', *, *, #9271, .F. ) ;
#6600 = DIRECTION ( 'NONE',  ( 1.000000000000000000, 0.000000000000000000, 0.000000000000000000 ) ) ;
#6601 = CARTESIAN_POINT ( 'NONE',  ( -2.343457872958619959, -1.451199717459270122, 4.916681529328610800 ) ) ;
#6602 = CARTESIAN_POINT ( 'NONE',  ( -2.180207327701300102, -5.506567796610169374, 5.586116916730199833 ) ) ;
#6603 = CARTESIAN_POINT ( 'NONE',  ( -1.373536515609910191, -1.218316834576379737, 6.970795264502737787 ) ) ;
#6604 = ORIENTED_EDGE ( 'NONE', *, *, #15171, .F. ) ;
#6605 = CARTESIAN_POINT ( 'NONE',  ( 1.399999999999999911, 0.5999999999999999778, 6.100000000000000533 ) ) ;
#6606 = CARTESIAN_POINT ( 'NONE',  ( 2.004091155098369104, -0.6361096273691766445, 4.254443623407341057 ) ) ;
#6607 = CARTESIAN_POINT ( 'NONE',  ( 1.882879255550339082, -0.4963798976394455664, 2.835213315261639000 ) ) ;
#6608 = DIRECTION ( 'NONE',  ( 2.379049338482479710E-16, 0.000000000000000000, 1.000000000000000000 ) ) ;
#6609 = LINE ( 'NONE', #5131, #7886 ) ;
#6610 = CARTESIAN_POINT ( 'NONE',  ( -2.050563521385710075, -4.595118636378185073, 4.800454404529219232 ) ) ;
#6611 = DIRECTION ( 'NONE',  ( -1.168655815394900078E-16, 1.000000000000000000, 5.843279076974510248E-17 ) ) ;
#6612 = CARTESIAN_POINT ( 'NONE',  ( 0.5999999999999999778, -7.347880794884110368E-17, 7.599999999999999645 ) ) ;
#6613 = CARTESIAN_POINT ( 'NONE',  ( 0.7368491673939637776, -3.523857375116919322, 2.783765372628159263 ) ) ;
#6614 = ORIENTED_EDGE ( 'NONE', *, *, #9737, .F. ) ;
#6615 = DIRECTION ( 'NONE',  ( 0.000000000000000000, 0.000000000000000000, 1.000000000000000000 ) ) ;
#6616 = CARTESIAN_POINT ( 'NONE',  ( -1.399999999999999911, 6.400000000000000355, 7.700000000000000178 ) ) ;
#6617 = CARTESIAN_POINT ( 'NONE',  ( 1.327748599278330000, -0.4480353997208159633, 2.745754414290000334 ) ) ;
#6618 = CARTESIAN_POINT ( 'NONE',  ( -1.524497189778160289, -2.801920438179980710, 6.872331008700187205 ) ) ;
#6619 = ORIENTED_EDGE ( 'NONE', *, *, #17391, .T. ) ;
#6620 = CARTESIAN_POINT ( 'NONE',  ( -0.5500000000000000444, 6.450000000000000178, 3.299999999999999822 ) ) ;
#6621 = LINE ( 'NONE', #11909, #18026 ) ;
#6622 = CARTESIAN_POINT ( 'NONE',  ( -2.041338374031088865, -5.219915254237295521, 4.918217215283674726 ) ) ;
#6623 = ORIENTED_EDGE ( 'NONE', *, *, #540, .F. ) ;
#6624 = EDGE_LOOP ( 'NONE', ( #13541, #17238, #14907, #5486 ) ) ;
#6625 = DIRECTION ( 'NONE',  ( 1.000000000000000000, 5.782411586589356455E-15, 3.614007241618347587E-15 ) ) ;
#6626 = AXIS2_PLACEMENT_3D ( 'NONE', #11026, #6862, #943 ) ;
#6627 = DIRECTION ( 'NONE',  ( 1.000000000000000000, 0.000000000000000000, 0.000000000000000000 ) ) ;
#6628 = CARTESIAN_POINT ( 'NONE',  ( -0.6207106781186549904, 3.050000000000000266, 2.628553390593269423 ) ) ;
#6629 = ORIENTED_EDGE ( 'NONE', *, *, #4770, .F. ) ;
#6630 = CARTESIAN_POINT ( 'NONE',  ( 0.4974685680287860290, -5.439830508474580384, 7.000224381598740386 ) ) ;
#6631 = CARTESIAN_POINT ( 'NONE',  ( 2.091881088960109825, -3.989623140882676555, 6.333140288723826394 ) ) ;
#6632 = CARTESIAN_POINT ( 'NONE',  ( -2.350000000000000089, -5.599999999999999645, 2.799999999999999822 ) ) ;
#6633 = CARTESIAN_POINT ( 'NONE',  ( -2.327043743583479429, -3.217268751009201289, 5.975923629552665872 ) ) ;
#6634 = LINE ( 'NONE', #14986, #8802 ) ;
#6635 = CARTESIAN_POINT ( 'NONE',  ( -0.06276132972181580616, -4.222506023765570049, 7.052616990284530374 ) ) ;
#6636 = EDGE_CURVE ( 'NONE', #9952, #3716, #9027, .T. ) ;
#6637 = PLANE ( 'NONE',  #12619 ) ;
#6638 = LINE ( 'NONE', #5159, #5593 ) ;
#6640 = EDGE_LOOP ( 'NONE', ( #2984, #12102, #3717, #4931 ) ) ;
#6639 = CARTESIAN_POINT ( 'NONE',  ( -0.2266049403550400299, -2.146007489747939090, 2.055805624768001216 ) ) ;
#6641 = EDGE_CURVE ( 'NONE', #6119, #4535, #13127, .T. ) ;
#6642 = EDGE_CURVE ( 'NONE', #17362, #16159, #11637, .T. ) ;
#6643 = FACE_OUTER_BOUND ( 'NONE', #673, .T. ) ;
#6644 = CARTESIAN_POINT ( 'NONE',  ( 2.270487904532159984, -0.3622881355932209835, 4.080813552109670894 ) ) ;
#6645 = CARTESIAN_POINT ( 'NONE',  ( -2.182690844914350059, -1.680241723982170088, 5.580117243900479806 ) ) ;
#6646 = CARTESIAN_POINT ( 'NONE',  ( -2.224278379903029901, -0.5091101694915259879, 5.468825643806110470 ) ) ;
#6647 = CARTESIAN_POINT ( 'NONE',  ( -1.217041937262000273, -0.2742238837839080512, 2.666998181419180547 ) ) ;
#6648 = CARTESIAN_POINT ( 'NONE',  ( -1.378221871957430178, -5.479872881355929870, 6.607619368096279366 ) ) ;
#6649 = ORIENTED_EDGE ( 'NONE', *, *, #8364, .F. ) ;
#6650 = DIRECTION ( 'NONE',  ( -2.986159789035700404E-15, 1.110223024625159992E-16, 1.000000000000000000 ) ) ;
#6651 = ORIENTED_EDGE ( 'NONE', *, *, #3722, .F. ) ;
#6652 = CARTESIAN_POINT ( 'NONE',  ( -1.000896394980329340, -5.170974576271190060, 6.829956240957378633 ) ) ;
#6653 = DIRECTION ( 'NONE',  ( -7.401486830834380223E-16, -1.769136588914770194E-30, 1.000000000000000000 ) ) ;
#6654 = CARTESIAN_POINT ( 'NONE',  ( 0.2335786437626899970, 6.450000000000000178, 1.958578643762689753 ) ) ;
#6655 = ORIENTED_EDGE ( 'NONE', *, *, #8689, .T. ) ;
#6656 = CARTESIAN_POINT ( 'NONE',  ( 0.8242394280877100021, -4.428259742000189902, 6.904399023015010073 ) ) ;
#6657 = EDGE_CURVE ( 'NONE', #1091, #12787, #16162, .T. ) ;
#6658 = CARTESIAN_POINT ( 'NONE',  ( -2.340070819011249803, -5.519915254237290014, 4.950151441910549899 ) ) ;
#6659 = CYLINDRICAL_SURFACE ( 'NONE', #7751, 0.04999999999999969746 ) ;
#6660 = ADVANCED_FACE ( 'NONE', ( #10237 ), #15909, .T. ) ;
#6661 = FACE_OUTER_BOUND ( 'NONE', #15607, .T. ) ;
#6662 = CARTESIAN_POINT ( 'NONE',  ( 0.2365712905368450025, -2.192584066324519743, 2.358466376073659720 ) ) ;
#6663 = EDGE_CURVE ( 'NONE', #6008, #14845, #11450, .T. ) ;
#6664 = FACE_OUTER_BOUND ( 'NONE', #3698, .T. ) ;
#6665 = CARTESIAN_POINT ( 'NONE',  ( -1.823404397755031159, -1.656953435693890864, 5.643450181448764980 ) ) ;
#6666 = LINE ( 'NONE', #17849, #11481 ) ;
#6667 = CARTESIAN_POINT ( 'NONE',  ( 1.248294325655350034, -0.3266949152542379942, 2.704938983774300088 ) ) ;
#6668 = CARTESIAN_POINT ( 'NONE',  ( -1.599999999999869971, 12.00000000000000000, 1.600000000000000089 ) ) ;
#6669 = VERTEX_POINT ( 'NONE', #8867 ) ;
#6670 = VECTOR ( 'NONE', #5394, 1000.000000000000000 ) ;
#6671 = LINE ( 'NONE', #13432, #15199 ) ;
#6672 = CARTESIAN_POINT ( 'NONE',  ( -1.670747221194377685, -5.103620102360557631, 3.047345349617607724 ) ) ;
#6673 = VERTEX_POINT ( 'NONE', #4689 ) ;
#6674 = VERTEX_POINT ( 'NONE', #14779 ) ;
#6675 = ORIENTED_EDGE ( 'NONE', *, *, #3008, .T. ) ;
#6676 = LINE ( 'NONE', #18125, #8617 ) ;
#6677 = CARTESIAN_POINT ( 'NONE',  ( -1.596341326794979976, -5.264406779661020330, 2.970780074643819990 ) ) ;
#6678 = PRODUCT ( 'Latch Lock Pin Wire', 'Latch Lock Pin Wire', '', ( #2047 ) ) ;
#6679 = CARTESIAN_POINT ( 'NONE',  ( 0.5500000000000000444, 0.5999999999999999778, 1.600000000000000089 ) ) ;
#6680 = DIRECTION ( 'NONE',  ( -2.220446049250309876E-16, 0.000000000000000000, 1.000000000000000000 ) ) ;
#6681 = VECTOR ( 'NONE', #1329, 1000.000000000000000 ) ;
#6682 = CARTESIAN_POINT ( 'NONE',  ( 2.161802606005190253, -0.5895330507925999886, 3.769755311421790545 ) ) ;
#6683 = ADVANCED_FACE ( 'NONE', ( #11916 ), #16007, .T. ) ;
#6684 = LINE ( 'NONE', #5482, #12043 ) ;
#6685 = CIRCLE ( 'NONE', #16744, 0.5000000000000000000 ) ;
#6686 = CARTESIAN_POINT ( 'NONE',  ( -2.004091155098381094, -4.963890372630814340, 4.254443623407394348 ) ) ;
#6687 = CARTESIAN_POINT ( 'NONE',  ( 0.1765068388402390998, -0.1468220338983061424, 7.347961541693647902 ) ) ;
#6688 = CARTESIAN_POINT ( 'NONE',  ( -2.351526912647309953, -0.5269067796610169552, 4.606040641882809261 ) ) ;
#6689 = CARTESIAN_POINT ( 'NONE',  ( -2.030998484741458832, -0.5180084745762725262, 4.999543428097190656 ) ) ;
#6690 = ORIENTED_EDGE ( 'NONE', *, *, #16927, .F. ) ;
#6691 = CARTESIAN_POINT ( 'NONE',  ( 0.4360591020457930123, -0.008898305084746040497, 2.387347919655840034 ) ) ;
#6692 = ORIENTED_EDGE ( 'NONE', *, *, #7219, .T. ) ;
#6693 = PLANE ( 'NONE',  #538 ) ;
#6694 = VECTOR ( 'NONE', #15112, 1000.000000000000000 ) ;
#6695 = CARTESIAN_POINT ( 'NONE',  ( 2.325590009395039903, -0.7292627805223300674, 5.061077271074019279 ) ) ;
#6696 =( NAMED_UNIT ( * ) SI_UNIT ( $, .STERADIAN. ) SOLID_ANGLE_UNIT ( ) );
#6697 = CARTESIAN_POINT ( 'NONE',  ( -1.378221871957430178, -5.479872881355929870, 6.607619368096279366 ) ) ;
#6698 = CARTESIAN_POINT ( 'NONE',  ( -2.370419177058770366, -1.358046564306109261, 5.893409660608596390 ) ) ;
#6699 = VERTEX_POINT ( 'NONE', #4774 ) ;
#6700 = CARTESIAN_POINT ( 'NONE',  ( -0.02999999999999379899, 12.00000000000000000, -2.869354249208270301E-17 ) ) ;
#6701 = ADVANCED_FACE ( 'NONE', ( #10425 ), #355, .T. ) ;
#6702 = CARTESIAN_POINT ( 'NONE',  ( -1.644832646965619816, -4.408812330071869567, 6.383232381746489992 ) ) ;
#6703 = AXIS2_PLACEMENT_3D ( 'NONE', #15292, #2604, #16753 ) ;
#6704 = CARTESIAN_POINT ( 'NONE',  ( 1.155768864438629695, -4.404971453711897134, 7.088998121597438029 ) ) ;
#6705 = EDGE_CURVE ( 'NONE', #12167, #12988, #14691, .T. ) ;
#6706 = CARTESIAN_POINT ( 'NONE',  ( -1.800000000000000044, 7.799999999999999822, 7.599999999999999645 ) ) ;
#6707 = LINE ( 'NONE', #16335, #13783 ) ;
#6708 = CARTESIAN_POINT ( 'NONE',  ( -1.199999999999869837, 12.00000000000000000, -2.399999999999999911 ) ) ;
#6709 = CARTESIAN_POINT ( 'NONE',  ( 2.033547680391670998, -0.9583047870452394701, 4.417890669792418734 ) ) ;
#6710 = CARTESIAN_POINT ( 'NONE',  ( -2.500000000000000000, 2.799999999999999822, 0.6099999999999999867 ) ) ;
#6711 = VECTOR ( 'NONE', #16455, 1000.000000000000000 ) ;
#6712 = VERTEX_POINT ( 'NONE', #16085 ) ;
#6713 = DIRECTION ( 'NONE',  ( 0.000000000000000000, 0.000000000000000000, 1.000000000000000000 ) ) ;
#6714 = VECTOR ( 'NONE', #275, 1000.000000000000000 ) ;
#6715 = DIRECTION ( 'NONE',  ( 0.000000000000000000, 6.123233995736769734E-17, -1.000000000000000000 ) ) ;
#6716 = CARTESIAN_POINT ( 'NONE',  ( -2.050059171113549183, -0.2224576271186441134, 4.809263467226075228 ) ) ;
#6717 = EDGE_CURVE ( 'NONE', #14300, #14847, #16853, .T. ) ;
#6718 = CARTESIAN_POINT ( 'NONE',  ( -1.094547058713670085, -2.755343861603408939, 7.117660114503937763 ) ) ;
#6719 = DIRECTION ( 'NONE',  ( 2.220446049250309876E-16, 1.000000000000000000, -1.850371707708599740E-16 ) ) ;
#6720 = AXIS2_PLACEMENT_3D ( 'NONE', #4580, #5246, #17728 ) ;
#6721 = CYLINDRICAL_SURFACE ( 'NONE', #6512, 0.6000000000000000888 ) ;
#6722 = CARTESIAN_POINT ( 'NONE',  ( -1.725722849164588624, -5.197669491525426011, 5.812007984777676661 ) ) ;
#6723 = ORIENTED_EDGE ( 'NONE', *, *, #3137, .T. ) ;
#6724 = LINE ( 'NONE', #7940, #3283 ) ;
#6725 = CARTESIAN_POINT ( 'NONE',  ( 2.224278379903029901, -5.390889830508481140, 5.468825643806100700 ) ) ;
#6726 = DIRECTION ( 'NONE',  ( 0.000000000000000000, 1.000000000000000000, 0.000000000000000000 ) ) ;
#6727 = ORIENTED_EDGE ( 'NONE', *, *, #510, .T. ) ;
#6728 = VECTOR ( 'NONE', #11344, 1000.000000000000000 ) ;
#6729 = CARTESIAN_POINT ( 'NONE',  ( 2.293398556041700065, -5.364194915254239859, 4.171956209133470317 ) ) ;
#6730 = VECTOR ( 'NONE', #6733, 1000.000000000000000 ) ;
#6731 = CARTESIAN_POINT ( 'NONE',  ( -2.510208264418979596, -4.525253771513313872, 5.561375738133230939 ) ) ;
#6732 = CARTESIAN_POINT ( 'NONE',  ( 1.370891210199511434, -3.869340823081269587, 2.427606771969341715 ) ) ;
#6733 = DIRECTION ( 'NONE',  ( 0.000000000000000000, -1.000000000000000000, -1.387778780781449866E-16 ) ) ;
#6734 = CARTESIAN_POINT ( 'NONE',  ( 0.2220816246932099114, -1.055298816558370101, 6.740975647723836950 ) ) ;
#6735 = VECTOR ( 'NONE', #1307, 1000.000000000000000 ) ;
#6736 = CIRCLE ( 'NONE', #18233, 1.016666666666670160 ) ;
#6737 = DIRECTION ( 'NONE',  ( -4.177994306516039113E-17, 0.7310552682428709259, -0.6823182503600090376 ) ) ;
#6738 = CARTESIAN_POINT ( 'NONE',  ( 0.1749999999999999889, 5.000000000000000000, -1.071565949253929989E-17 ) ) ;
#6739 = ORIENTED_EDGE ( 'NONE', *, *, #8168, .T. ) ;
#6740 = EDGE_CURVE ( 'NONE', #10826, #14727, #619, .T. ) ;
#6741 = VECTOR ( 'NONE', #2092, 1000.000000000000000 ) ;
#6742 = CARTESIAN_POINT ( 'NONE',  ( 1.716288473737299869, -5.318200384451399643, 2.983711526262690317 ) ) ;
#6743 = CARTESIAN_POINT ( 'NONE',  ( -2.293398556041709835, -0.5358050847457630494, 4.171956209133480975 ) ) ;
#6744 = CARTESIAN_POINT ( 'NONE',  ( -0.6343239990445920240, -2.099430913171359769, 2.433641963034089972 ) ) ;
#6745 = CARTESIAN_POINT ( 'NONE',  ( -1.899999999999999911, 9.199999999999999289, 0.5999999999999999778 ) ) ;
#6746 = CARTESIAN_POINT ( 'NONE',  ( -1.661700935788390066, -0.4124999999999999778, 3.038299064211610112 ) ) ;
#6747 = CARTESIAN_POINT ( 'NONE',  ( 0.5609751937345880402, -5.439830508474575943, 7.293870047334757523 ) ) ;
#6748 = ORIENTED_EDGE ( 'NONE', *, *, #2958, .F. ) ;
#6749 = PLANE ( 'NONE',  #15859 ) ;
#6750 = CARTESIAN_POINT ( 'NONE',  ( 0.007887181101542477604, -0.3249948581819089855, 2.435887274406100200 ) ) ;
#6751 = AXIS2_PLACEMENT_3D ( 'NONE', #9314, #13492, #13596 ) ;
#6752 = ADVANCED_FACE ( 'NONE', ( #16170 ), #3474, .T. ) ;
#6753 = VECTOR ( 'NONE', #9628, 1000.000000000000000 ) ;
#6754 = ORIENTED_EDGE ( 'NONE', *, *, #536, .T. ) ;
#6755 = EDGE_CURVE ( 'NONE', #10460, #14390, #10616, .T. ) ;
#6756 = CARTESIAN_POINT ( 'NONE',  ( 0.8189529353761060282, -3.822764246504690266, 2.493631540942729874 ) ) ;
#6757 = VECTOR ( 'NONE', #11034, 1000.000000000000000 ) ;
#6758 = CIRCLE ( 'NONE', #1450, 0.04999999999999991257 ) ;
#6759 = CARTESIAN_POINT ( 'NONE',  ( 0.9150601050661639757, -5.430932203389830626, 6.868218666554230190 ) ) ;
#6760 = CARTESIAN_POINT ( 'NONE',  ( -1.250000000000000000, 3.500000000000000000, 6.100000000000000533 ) ) ;
#6761 = DIRECTION ( 'NONE',  ( 1.224646799147350002E-16, -1.000000000000000000, -6.123233995736769734E-17 ) ) ;
#6762 = CARTESIAN_POINT ( 'NONE',  ( -2.111627294540180166, -1.889836318576769925, 3.660877362176710559 ) ) ;
#6763 = AXIS2_PLACEMENT_3D ( 'NONE', #17609, #17235, #11803 ) ;
#6764 = CARTESIAN_POINT ( 'NONE',  ( -1.485788269501199910, -4.829629811528119987, 2.863981322975840182 ) ) ;
#6765 = AXIS2_PLACEMENT_3D ( 'NONE', #17835, #9618, #12490 ) ;
#6766 = CARTESIAN_POINT ( 'NONE',  ( -1.353302556710470395, -1.563800282540731779, 6.243850391919187892 ) ) ;
#6767 = CARTESIAN_POINT ( 'NONE',  ( 0.1749999999999999889, 9.299999999999998934, 0.5999999999999999778 ) ) ;
#6768 = DIRECTION ( 'NONE',  ( -0.9622640697945192834, -0.2721173643531200614, 0.000000000000000000 ) ) ;
#6769 = VERTEX_POINT ( 'NONE', #9215 ) ;
#6770 = ADVANCED_FACE ( 'NONE', ( #14879 ), #7395, .T. ) ;
#6771 = CARTESIAN_POINT ( 'NONE',  ( 0.1749999999999999889, 9.299999999999998934, 0.4000000000000000222 ) ) ;
#6772 = CARTESIAN_POINT ( 'NONE',  ( 0.1749999999999999889, 2.700000000000000178, 1.600000000000000089 ) ) ;
#6773 = VERTEX_POINT ( 'NONE', #8123 ) ;
#6774 = ADVANCED_FACE ( 'NONE', ( #904 ), #17812, .T. ) ;
#6775 = PRODUCT_DEFINITION_CONTEXT ( 'detailed design', #17577, 'design' ) ;
#6776 = ADVANCED_FACE ( 'NONE', ( #10799 ), #10903, .T. ) ;
#6777 = ORIENTED_EDGE ( 'NONE', *, *, #6755, .T. ) ;
#6778 = CARTESIAN_POINT ( 'NONE',  ( 1.699999999999999956, 2.299999999999999822, 7.599999999999999645 ) ) ;
#6779 = EDGE_CURVE ( 'NONE', #16856, #356, #6542, .T. ) ;
#6780 = AXIS2_PLACEMENT_3D ( 'NONE', #14317, #11711, #7544 ) ;
#6781 = CARTESIAN_POINT ( 'NONE',  ( -0.8570167067220350043, -5.282203389830510076, 2.508190348879359988 ) ) ;
#6782 = EDGE_CURVE ( 'NONE', #16101, #9670, #13759, .T. ) ;
#6783 = EDGE_CURVE ( 'NONE', #16266, #10138, #11739, .T. ) ;
#6784 = PLANE ( 'NONE',  #7887 ) ;
#6785 = LINE ( 'NONE', #7893, #809 ) ;
#6786 = CARTESIAN_POINT ( 'NONE',  ( -2.111627294540180166, -1.889836318576769925, 3.660877362176710559 ) ) ;
#6787 = CARTESIAN_POINT ( 'NONE',  ( -2.578017356471871135, -0.2135593220338991571, 5.329826563567776176 ) ) ;
#6788 = ORIENTED_EDGE ( 'NONE', *, *, #15164, .T. ) ;
#6789 = FACE_OUTER_BOUND ( 'NONE', #12000, .T. ) ;
#6790 = VECTOR ( 'NONE', #16624, 1000.000000000000000 ) ;
#6791 = ORIENTED_EDGE ( 'NONE', *, *, #2571, .T. ) ;
#6792 = CARTESIAN_POINT ( 'NONE',  ( 1.925836318347889931, -0.1112288135593229726, 6.525927015348126581 ) ) ;
#6793 = CARTESIAN_POINT ( 'NONE',  ( 1.750000000000000000, 0.5999999999999999778, 7.599999999999999645 ) ) ;
#6794 = ORIENTED_EDGE ( 'NONE', *, *, #16940, .T. ) ;
#6795 = DIRECTION ( 'NONE',  ( 0.000000000000000000, 1.110223024625159992E-16, -1.000000000000000000 ) ) ;
#6796 = ADVANCED_FACE ( 'NONE', ( #12381 ), #14977, .T. ) ;
#6797 = CARTESIAN_POINT ( 'NONE',  ( 0.04278372834676708036, -1.870388906648450478, 2.346934926511239805 ) ) ;
#6798 = CARTESIAN_POINT ( 'NONE',  ( 0.000000000000000000, 0.000000000000000000, 0.000000000000000000 ) ) ;
#6799 = CARTESIAN_POINT ( 'NONE',  ( -2.318251751302029984, -5.533262711864409766, 4.294764266798999586 ) ) ;
#6800 = CARTESIAN_POINT ( 'NONE',  ( 2.437122747866759198, -0.5895330507926000996, 3.649501829874934433 ) ) ;
#6801 = VERTEX_POINT ( 'NONE', #798 ) ;
#6802 = CARTESIAN_POINT ( 'NONE',  ( -0.5902886515192680150, -1.447358841099289917, 6.978224088050050788 ) ) ;
#6803 = VECTOR ( 'NONE', #2313, 1000.000000000000000 ) ;
#6804 = CARTESIAN_POINT ( 'NONE',  ( 1.990095963740240004, -0.7525510688106187285, 5.204400533041760646 ) ) ;
#6805 = CARTESIAN_POINT ( 'NONE',  ( 2.328527996529149657, -0.5662447625043111055, 3.426787111016343701 ) ) ;
#6806 = LINE ( 'NONE', #12363, #14984 ) ;
#6807 = CARTESIAN_POINT ( 'NONE',  ( -1.399999999999999911, -7.000000000000000000, 6.100000000000000533 ) ) ;
#6808 = FACE_OUTER_BOUND ( 'NONE', #16571, .T. ) ;
#6809 = CARTESIAN_POINT ( 'NONE',  ( -1.572563554680370679, -4.781424942684484591, 3.380172092915589843 ) ) ;
#6810 = LINE ( 'NONE', #12547, #10865 ) ;
#6811 = ADVANCED_FACE ( 'NONE', ( #18003 ), #2478, .T. ) ;
#6812 = ORIENTED_EDGE ( 'NONE', *, *, #14840, .T. ) ;
#6813 = DIRECTION ( 'NONE',  ( -0.7071067811865470176, -0.7071067811865480168, 0.000000000000000000 ) ) ;
#6814 = DIRECTION ( 'NONE',  ( 1.000000000000000000, 0.000000000000000000, 0.000000000000000000 ) ) ;
#6815 = CARTESIAN_POINT ( 'NONE',  ( 1.883442729065728960, -2.452596113855660676, 6.569694408006650832 ) ) ;
#6816 = VERTEX_POINT ( 'NONE', #5347 ) ;
#6817 = VECTOR ( 'NONE', #6168, 1000.000000000000000 ) ;
#6818 = PLANE ( 'NONE',  #2585 ) ;
#6819 = CARTESIAN_POINT ( 'NONE',  ( -0.1914205519645679199, -4.981295943764795453, 2.049234377954000319 ) ) ;
#6820 = CARTESIAN_POINT ( 'NONE',  ( 1.869504824896970119, -5.395338983050850246, 5.548311746956850143 ) ) ;
#6821 = VERTEX_POINT ( 'NONE', #12469 ) ;
#6822 = EDGE_CURVE ( 'NONE', #16560, #13202, #8210, .T. ) ;
#6823 = DIRECTION ( 'NONE',  ( -1.000000000000000000, -1.306144734853129823E-16, 0.000000000000000000 ) ) ;
#6824 = CARTESIAN_POINT ( 'NONE',  ( -1.800000000000000044, 12.00000000000000000, 7.649999999999999467 ) ) ;
#6825 = DIRECTION ( 'NONE',  ( 1.000000000000000000, 0.000000000000000000, 0.000000000000000000 ) ) ;
#6826 = VERTEX_POINT ( 'NONE', #8040 ) ;
#6827 = CARTESIAN_POINT ( 'NONE',  ( -0.06367493584607197832, -5.598516949152545941, 2.649999999999998579 ) ) ;
#6828 = CARTESIAN_POINT ( 'NONE',  ( 0.1785884594055070773, -4.199217735477280833, 7.347870815423032553 ) ) ;
#6829 = CARTESIAN_POINT ( 'NONE',  ( 2.653886076156968699, -4.125511994252439862, 4.698454755023375284 ) ) ;
#6830 = DIRECTION ( 'NONE',  ( -1.000000000000000000, -1.110223024625159992E-16, 1.110223024625159992E-16 ) ) ;
#6831 = VECTOR ( 'NONE', #8481, 1000.000000000000000 ) ;
#6832 = CARTESIAN_POINT ( 'NONE',  ( -2.351212046067109984, -4.618406924666470736, 4.597298481426070893 ) ) ;
#6833 = CARTESIAN_POINT ( 'NONE',  ( -1.699999999999999956, 9.299999999999998934, 7.700000000000000178 ) ) ;
#6834 = VERTEX_POINT ( 'NONE', #16355 ) ;
#6835 = VECTOR ( 'NONE', #12583, 1000.000000000000114 ) ;
#6836 = CARTESIAN_POINT ( 'NONE',  ( 1.671117483942869963, -5.337498512511849924, 3.028882516057120000 ) ) ;
#6837 = CARTESIAN_POINT ( 'NONE',  ( 0.7983658734558030101, -0.4334745762711870176, 6.913847129767330735 ) ) ;
#6838 = CARTESIAN_POINT ( 'NONE',  ( -1.669205944673819886, -3.147403886144329643, 6.359065158982450505 ) ) ;
#6839 = DIRECTION ( 'NONE',  ( -1.000000000000000000, 0.000000000000000000, -3.700743415417190112E-16 ) ) ;
#6840 = CARTESIAN_POINT ( 'NONE',  ( -6.123233995736763571E-17, 5.318248954186070243, 6.899999999999999467 ) ) ;
#6841 = CARTESIAN_POINT ( 'NONE',  ( -1.347262683220810553, -5.475423728813556323, 6.986424775243341045 ) ) ;
#6842 = VERTEX_POINT ( 'NONE', #3660 ) ;
#6843 = PRODUCT_DEFINITION_SHAPE ( 'NONE', 'NONE',  #15039 ) ;
#6844 = ORIENTED_EDGE ( 'NONE', *, *, #11653, .T. ) ;
#6845 = CARTESIAN_POINT ( 'NONE',  ( 2.058670345754649134, -5.050847457627118509, 3.559656372813920111 ) ) ;
#6846 = DIRECTION ( 'NONE',  ( -2.168404344971021884E-15, 1.000000000000000000, 0.000000000000000000 ) ) ;
#6847 = CARTESIAN_POINT ( 'NONE',  ( 6.429395695523600208E-16, 3.500000000000000000, 5.100000000000000533 ) ) ;
#6848 = EDGE_LOOP ( 'NONE', ( #10132, #6971, #966, #17283 ) ) ;
#6849 = CARTESIAN_POINT ( 'NONE',  ( -1.781655196750479897, -3.520016498756949996, 3.162323035427820450 ) ) ;
#6850 = DIRECTION ( 'NONE',  ( 1.059965646700398694E-16, 0.6823182503600109250, 0.7310552682428693716 ) ) ;
#6851 = CARTESIAN_POINT ( 'NONE',  ( 1.487835687536851470, -5.028306595106930565, 2.490167689244129789 ) ) ;
#6852 = DIRECTION ( 'NONE',  ( 0.000000000000000000, -1.000000000000000000, -6.167905692361979821E-17 ) ) ;
#6853 = CARTESIAN_POINT ( 'NONE',  ( 2.350000000000000089, -6.000000000000000000, 6.400000000000000355 ) ) ;
#6854 = CARTESIAN_POINT ( 'NONE',  ( 0.8189529353761060282, -3.822764246504690266, 2.493631540942729874 ) ) ;
#6855 = CYLINDRICAL_SURFACE ( 'NONE', #184, 0.09999999999999997780 ) ;
#6856 = CARTESIAN_POINT ( 'NONE',  ( 0.4874850653660255384, -2.891232714973161144, 6.694306935672937442 ) ) ;
#6857 = CARTESIAN_POINT ( 'NONE',  ( -0.9150601050661559821, -0.4690677966101700069, 6.868218666554230190 ) ) ;
#6858 = CARTESIAN_POINT ( 'NONE',  ( 1.875000000000000000, 12.00000000000000000, 7.700000000000000178 ) ) ;
#6859 = CARTESIAN_POINT ( 'NONE',  ( 1.399999999999999911, -6.000000000000000000, 3.299999999999999822 ) ) ;
#6860 = ORIENTED_EDGE ( 'NONE', *, *, #5956, .T. ) ;
#6861 = APPLICATION_CONTEXT ( 'automotive_design' ) ;
#6862 = DIRECTION ( 'NONE',  ( 0.000000000000000000, 0.000000000000000000, -1.000000000000000000 ) ) ;
#6863 = ORIENTED_EDGE ( 'NONE', *, *, #13276, .T. ) ;
#6864 = VERTEX_POINT ( 'NONE', #10991 ) ;
#6865 = EDGE_LOOP ( 'NONE', ( #1623, #11346, #8842, #11336 ) ) ;
#6866 = CARTESIAN_POINT ( 'NONE',  ( 1.850000000000000089, 11.25000000000000000, 8.300000000000000711 ) ) ;
#6867 = CARTESIAN_POINT ( 'NONE',  ( -1.921786527979019166, -5.242161016949150820, 3.977907449687794195 ) ) ;
#6868 = CARTESIAN_POINT ( 'NONE',  ( -1.899999999999999911, 2.000000000000000000, 1.600000000000000089 ) ) ;
#6869 = CARTESIAN_POINT ( 'NONE',  ( 0.3750000000000000000, 6.450000000000000178, 2.100000000000000089 ) ) ;
#6870 = CARTESIAN_POINT ( 'NONE',  ( 2.500000000000000000, 10.00000000000000000, 1.600000000000000089 ) ) ;
#6871 = CARTESIAN_POINT ( 'NONE',  ( -1.695999708020951013, -5.128627060139315574, 2.646274854235481921 ) ) ;
#6872 = ADVANCED_FACE ( 'NONE', ( #5149 ), #13682, .F. ) ;
#6873 = DIRECTION ( 'NONE',  ( -1.586032892321649771E-16, 0.000000000000000000, -1.000000000000000000 ) ) ;
#6874 = CARTESIAN_POINT ( 'NONE',  ( -1.854177340199669954, -1.610376859117309989, 6.149404042554720284 ) ) ;
#6875 = EDGE_CURVE ( 'NONE', #2335, #7455, #7942, .T. ) ;
#6876 = CARTESIAN_POINT ( 'NONE',  ( -2.171642826483958899, -0.1957627118644069686, 6.225392547715731695 ) ) ;
#6877 = CARTESIAN_POINT ( 'NONE',  ( -1.477796163681079911, -0.4824152542372879826, 6.531563725478150673 ) ) ;
#6878 = EDGE_CURVE ( 'NONE', #10219, #16165, #1177, .T. ) ;
#6879 = EDGE_CURVE ( 'NONE', #1517, #4371, #4028, .T. ) ;
#6880 = ORIENTED_EDGE ( 'NONE', *, *, #14712, .T. ) ;
#6881 = CARTESIAN_POINT ( 'NONE',  ( -0.9150601050661559821, -0.1690677966101700180, 6.868218666554230190 ) ) ;
#6882 = CARTESIAN_POINT ( 'NONE',  ( 1.803891155489780074, -0.8185750573155089471, 3.188470185434109982 ) ) ;
#6883 = ORIENTED_EDGE ( 'NONE', *, *, #639, .F. ) ;
#6884 = DIRECTION ( 'NONE',  ( -2.242874797222539596E-16, 0.000000000000000000, -1.000000000000000000 ) ) ;
#6885 = CARTESIAN_POINT ( 'NONE',  ( -1.687170344131989630, -2.848497014756560919, 6.340793075730589479 ) ) ;
#6886 = CARTESIAN_POINT ( 'NONE',  ( -1.347262683220810553, -5.475423728813556323, 6.986424775243341045 ) ) ;
#6887 = ORIENTED_EDGE ( 'NONE', *, *, #6537, .F. ) ;
#6888 = CARTESIAN_POINT ( 'NONE',  ( -1.710920205120030069, -1.587088570829020107, 6.316012914303580139 ) ) ;
#6889 = VECTOR ( 'NONE', #5448, 1000.000000000000000 ) ;
#6890 = CARTESIAN_POINT ( 'NONE',  ( 1.503462833636809881, -0.5041426604022095637, 3.304888304972889657 ) ) ;
#6891 = VERTEX_POINT ( 'NONE', #6628 ) ;
#6892 = LINE ( 'NONE', #14106, #17605 ) ;
#6893 = LINE ( 'NONE', #18153, #5986 ) ;
#6894 = FACE_OUTER_BOUND ( 'NONE', #11682, .T. ) ;
#6895 = CARTESIAN_POINT ( 'NONE',  ( 1.876226141297899774, -0.8884399221803740421, 3.866526959224306115 ) ) ;
#6897 = ADVANCED_FACE ( 'NONE', ( #12285 ), #16550, .T. ) ;
#6896 = CARTESIAN_POINT ( 'NONE',  ( 1.800000000000000044, 0.5999999999999999778, 7.550000000000000711 ) ) ;
#6898 = ORIENTED_EDGE ( 'NONE', *, *, #8575, .T. ) ;
#6899 = DIRECTION ( 'NONE',  ( -0.7071067811865470176, -0.7071067811865480168, 0.000000000000000000 ) ) ;
#6900 = LINE ( 'NONE', #12550, #11765 ) ;
#6901 = CARTESIAN_POINT ( 'NONE',  ( -1.695509042132779864, -0.2536016949152540834, 3.542446458728619518 ) ) ;
#6902 = CARTESIAN_POINT ( 'NONE',  ( 2.479511223993269287, -3.733451969711523155, 3.753882785753661633 ) ) ;
#6903 = AXIS2_PLACEMENT_3D ( 'NONE', #9114, #4766, #17528 ) ;
#6904 = VERTEX_POINT ( 'NONE', #15253 ) ;
#6905 = CARTESIAN_POINT ( 'NONE',  ( -1.882879255550339082, -5.103620102360555855, 2.835213315261639000 ) ) ;
#6906 = CARTESIAN_POINT ( 'NONE',  ( -0.8731223871104993872, -5.170974576271189171, 6.558046933601121786 ) ) ;
#6907 = ORIENTED_EDGE ( 'NONE', *, *, #16883, .F. ) ;
#6908 = CARTESIAN_POINT ( 'NONE',  ( 1.549742865090599997, -0.1156779661016950206, 6.471102547561450535 ) ) ;
#6909 = CARTESIAN_POINT ( 'NONE',  ( 1.875000000000000000, 11.25000000000000000, 7.700000000000000178 ) ) ;
#6910 = FACE_OUTER_BOUND ( 'NONE', #15910, .T. ) ;
#6911 = VERTEX_POINT ( 'NONE', #8580 ) ;
#6912 = CARTESIAN_POINT ( 'NONE',  ( -0.2189795514005259958, -5.595550847457629651, 2.356806637999020015 ) ) ;
#6913 = CARTESIAN_POINT ( 'NONE',  ( -1.032615103526609568, -4.315659176918716255, 7.144753513336388195 ) ) ;
#6914 = CARTESIAN_POINT ( 'NONE',  ( 2.642175029090480631, -4.102223705964154199, 4.450952196049445142 ) ) ;
#6915 = DIRECTION ( 'NONE',  ( 0.000000000000000000, -4.482164234210289821E-32, -1.000000000000000000 ) ) ;
#6916 = CARTESIAN_POINT ( 'NONE',  ( -1.936998685628559924, -4.758136654396199816, 3.363294429306559863 ) ) ;
#6918 = ADVANCED_FACE ( 'NONE', ( #6910 ), #8483, .T. ) ;
#6917 = DIRECTION ( 'NONE',  ( 1.903239470785979823E-16, 1.000000000000000000, 0.000000000000000000 ) ) ;
#6919 = ORIENTED_EDGE ( 'NONE', *, *, #15261, .F. ) ;
#6920 = CARTESIAN_POINT ( 'NONE',  ( 1.800000000000000044, 0.5999999999999999778, 7.599999999999999645 ) ) ;
#6921 = CARTESIAN_POINT ( 'NONE',  ( -0.4974685680287780354, -0.4601694915254240237, 7.000224381598740386 ) ) ;
#6922 = CARTESIAN_POINT ( 'NONE',  ( 2.245209214543399945, -2.635061543801989981, 5.405536158119010004 ) ) ;
#6923 = LINE ( 'NONE', #13960, #12506 ) ;
#6924 = LINE ( 'NONE', #16831, #8290 ) ;
#6925 = CARTESIAN_POINT ( 'NONE',  ( 2.651721837666119796, -5.073093220338980025, 4.594045830208265180 ) ) ;
#6926 = ORIENTED_EDGE ( 'NONE', *, *, #187, .F. ) ;
#6927 = VERTEX_POINT ( 'NONE', #1631 ) ;
#6928 = FACE_OUTER_BOUND ( 'NONE', #691, .T. ) ;
#6929 = DIRECTION ( 'NONE',  ( -2.220446049250309876E-16, -1.000000000000000000, 0.000000000000000000 ) ) ;
#6930 = CARTESIAN_POINT ( 'NONE',  ( -0.009452110982655708218, -0.5998079552954630467, 2.350000000000000089 ) ) ;
#6931 = ORIENTED_EDGE ( 'NONE', *, *, #15715, .T. ) ;
#6932 = CARTESIAN_POINT ( 'NONE',  ( 1.567709126316360058, -3.915917399657849796, 2.944712621036570166 ) ) ;
#6933 = SURFACE_SIDE_STYLE ('',( #5733 ) ) ;
#6934 = CARTESIAN_POINT ( 'NONE',  ( 0.2270348434643680025, -5.304612347394249916, 2.348896311281980065 ) ) ;
#6935 = CARTESIAN_POINT ( 'NONE',  ( -0.5999999999999999778, 0.5999999999999999778, 7.599999999999999645 ) ) ;
#6937 = EDGE_CURVE ( 'NONE', #11364, #2762, #11356, .T. ) ;
#6936 = DIRECTION ( 'NONE',  ( -1.224646799147350002E-16, 1.000000000000000000, 6.123233995736759873E-17 ) ) ;
#6938 = CARTESIAN_POINT ( 'NONE',  ( -0.2564439965878500538, -4.544701183441629766, 7.039440566481220074 ) ) ;
#6939 = LINE ( 'NONE', #12586, #2254 ) ;
#6940 = CARTESIAN_POINT ( 'NONE',  ( -0.7854158957162378218, -3.636457940198391636, 2.803154272645148826 ) ) ;
#6941 = PLANE ( 'NONE',  #9966 ) ;
#6942 = ORIENTED_EDGE ( 'NONE', *, *, #3966, .T. ) ;
#6943 = LINE ( 'NONE', #8620, #12423 ) ;
#6944 = EDGE_LOOP ( 'NONE', ( #13956, #15810, #11262, #15555 ) ) ;
#6945 = CARTESIAN_POINT ( 'NONE',  ( -2.352190863465239978, -4.917313796054239461, 4.622903765856379188 ) ) ;
#6946 = ORIENTED_EDGE ( 'NONE', *, *, #15234, .T. ) ;
#6947 = ORIENTED_EDGE ( 'NONE', *, *, #13946, .F. ) ;
#6948 = B_SPLINE_CURVE_WITH_KNOTS ( 'NONE', 3,
 ( #1781, #2996, #15952, #387, #5941, #11672, #17130, #6027, #15588, #2902, #4533, #17297, #11501, #3252, #8896, #14544 ),
 .UNSPECIFIED., .F., .F.,
 ( 4, 1, 1, 1, 1, 1, 1, 1, 1, 1, 1, 1, 1, 4 ),
 ( 0.4999998212288473409, 0.5105793490763189668, 0.5531463519624459924, 0.5957147871421379914, 0.6382850093031660066, 0.6808567369984199757, 0.7234300338917259987, 0.7660011046591950201, 0.8085801951440879654, 0.8511153557611940146, 0.8935297551198210231, 0.9363130006847799613, 0.9717764100584680431, 1.000000000000000000 ),
 .UNSPECIFIED. ) ;
#6949 = UNCERTAINTY_MEASURE_WITH_UNIT (LENGTH_MEASURE( 1.000000000000000082E-05 ), #294, 'distance_accuracy_value', 'NONE');
#6950 = VERTEX_POINT ( 'NONE', #14127 ) ;
#6951 = LINE ( 'NONE', #4169, #10366 ) ;
#6952 = CARTESIAN_POINT ( 'NONE',  ( -1.901882987994748975, -5.206567796610170440, 5.472995608211450147 ) ) ;
#6953 = CARTESIAN_POINT ( 'NONE',  ( -2.369027826908540302, -1.590929447188999646, 3.503830760997904470 ) ) ;
#6954 = DIRECTION ( 'NONE',  ( 1.233581138472399909E-16, 6.167905692361979821E-17, -1.000000000000000000 ) ) ;
#6955 = PLANE ( 'NONE',  #14115 ) ;
#6956 = VECTOR ( 'NONE', #10692, 1000.000000000000000 ) ;
#6957 = CARTESIAN_POINT ( 'NONE',  ( 1.399999999999999911, 6.400000000000000355, 7.700000000000000178 ) ) ;
#6958 = LINE ( 'NONE', #18049, #14091 ) ;
#6959 = DIRECTION ( 'NONE',  ( 1.110223024625159992E-16, 0.000000000000000000, -1.000000000000000000 ) ) ;
#6960 = CARTESIAN_POINT ( 'NONE',  ( 0.06276132972186961034, -1.377493976234430040, 7.052616990284530374 ) ) ;
#6961 = CARTESIAN_POINT ( 'NONE',  ( -0.4874850653659789645, -2.708767285026830951, 6.694306935672950765 ) ) ;
#6962 = CARTESIAN_POINT ( 'NONE',  ( 0.3803919826356921829, -0.008898305084746057844, 2.682580100125298461 ) ) ;
#6963 = ORIENTED_EDGE ( 'NONE', *, *, #13850, .T. ) ;
#6964 = CARTESIAN_POINT ( 'NONE',  ( 0.7983658734558030101, -0.4334745762711870176, 6.913847129767330735 ) ) ;
#6965 = DIRECTION ( 'NONE',  ( 2.220446049250309876E-16, 1.000000000000000000, 1.841437368383549833E-16 ) ) ;
#6966 = ORIENTED_EDGE ( 'NONE', *, *, #15845, .F. ) ;
#6967 = CARTESIAN_POINT ( 'NONE',  ( 1.378221871957440170, -0.1201271186440679983, 6.607619368096269596 ) ) ;
#6968 = CARTESIAN_POINT ( 'NONE',  ( 1.303621121494459967, -1.237764246504700072, 6.659417683669679455 ) ) ;
#6969 = ORIENTED_EDGE ( 'NONE', *, *, #5895, .T. ) ;
#6970 = DIRECTION ( 'NONE',  ( 0.7071067811865480168, 0.7071067811865470176, 0.000000000000000000 ) ) ;
#6971 = ORIENTED_EDGE ( 'NONE', *, *, #15217, .F. ) ;
#6972 = CARTESIAN_POINT ( 'NONE',  ( 1.145304265383909836, -2.522460978720528768, 6.755972720436078660 ) ) ;
#6973 = CARTESIAN_POINT ( 'NONE',  ( -0.4221287159901280228, -5.457627118644064801, 7.320050063945812369 ) ) ;
#6974 = VECTOR ( 'NONE', #10834, 1000.000000000000000 ) ;
#6975 = ADVANCED_FACE ( 'NONE', ( #248 ), #15630, .T. ) ;
#6976 = ORIENTED_EDGE ( 'NONE', *, *, #15995, .T. ) ;
#6977 = CARTESIAN_POINT ( 'NONE',  ( 2.151546283159470274, -0.8884399221803740421, 3.746273477677459773 ) ) ;
#6978 = ADVANCED_FACE ( 'NONE', ( #1454 ), #7111, .T. ) ;
#6979 = CARTESIAN_POINT ( 'NONE',  ( 1.428515267734870031, -0.3311440677966109858, 2.829745655876919841 ) ) ;
#6980 = ORIENTED_EDGE ( 'NONE', *, *, #15750, .T. ) ;
#6981 = CARTESIAN_POINT ( 'NONE',  ( 0.1749999999999999889, 7.700000000000000178, 1.600000000000000089 ) ) ;
#6982 = LINE ( 'NONE', #4288, #14550 ) ;
#6983 = DIRECTION ( 'NONE',  ( 3.700743415417199972E-16, -1.000000000000000000, -3.581736239852560511E-31 ) ) ;
#6984 = CARTESIAN_POINT ( 'NONE',  ( 1.683529720875211799, -1.144611093351550091, 5.875001924065625936 ) ) ;
#6985 = PRODUCT_DEFINITION_SHAPE ( 'NONE', 'NONE',  #4382 ) ;
#6986 = DIRECTION ( 'NONE',  ( 1.025799815460950140E-14, 1.000000000000000000, 0.000000000000000000 ) ) ;
#6987 = CARTESIAN_POINT ( 'NONE',  ( 0.08231150243515643339, -0.3014830508474583004, 2.050000000000001155 ) ) ;
#6988 = AXIS2_PLACEMENT_3D ( 'NONE', #4260, #14273, #16769 ) ;
#6989 = ORIENTED_EDGE ( 'NONE', *, *, #2845, .F. ) ;
#6990 = DIRECTION ( 'NONE',  ( -1.306144734853125878E-16, 1.000000000000000000, 0.000000000000000000 ) ) ;
#6991 = DIRECTION ( 'NONE',  ( 0.000000000000000000, 0.000000000000000000, -1.000000000000000000 ) ) ;
#6992 = CARTESIAN_POINT ( 'NONE',  ( -0.05465110135555984600, -0.1512711864406780515, 6.752241303418941243 ) ) ;
#6993 = AXIS2_PLACEMENT_3D ( 'NONE', #5465, #3974, #3796 ) ;
#6994 = AXIS2_PLACEMENT_3D ( 'NONE', #6981, #11054, #2823 ) ;
#6995 = CARTESIAN_POINT ( 'NONE',  ( 2.091881088960109825, -3.989623140882676555, 6.333140288723826394 ) ) ;
#6996 = ORIENTED_EDGE ( 'NONE', *, *, #15711, .T. ) ;
#6997 = CARTESIAN_POINT ( 'NONE',  ( -1.314185150718290895, -5.128627060139315574, 3.113044112970123400 ) ) ;
#6998 = CARTESIAN_POINT ( 'NONE',  ( -0.5664586606772434862, -5.286652542372874741, 2.726727161522279452 ) ) ;
#6999 = ORIENTED_EDGE ( 'NONE', *, *, #6353, .F. ) ;
#7000 = EDGE_CURVE ( 'NONE', #3076, #4272, #12653, .T. ) ;
#7001 = CARTESIAN_POINT ( 'NONE',  ( 1.596341326794970206, -0.03559322033898329463, 2.970780074643810664 ) ) ;
#7002 = CARTESIAN_POINT ( 'NONE',  ( 1.906474350327903052E-15, 10.16754446796632649, 7.700000000000000178 ) ) ;
#7003 = FACE_OUTER_BOUND ( 'NONE', #16438, .T. ) ;
#7004 = EDGE_CURVE ( 'NONE', #6826, #1785, #16990, .T. ) ;
#7005 = VERTEX_POINT ( 'NONE', #5887 ) ;
#7006 = DIRECTION ( 'NONE',  ( 0.000000000000000000, 0.000000000000000000, -1.000000000000000000 ) ) ;
#7007 = EDGE_CURVE ( 'NONE', #13279, #4421, #4303, .T. ) ;
#7008 = CARTESIAN_POINT ( 'NONE',  ( 1.914021115237030113, -0.8457042219637709302, 6.069404563272200015 ) ) ;
#7009 = EDGE_CURVE ( 'NONE', #16249, #13226, #10534, .T. ) ;
#7010 = VECTOR ( 'NONE', #1184, 1000.000000000000000 ) ;
#7011 = DIRECTION ( 'NONE',  ( -1.224646799147350002E-16, 1.000000000000000000, 6.123233995736769734E-17 ) ) ;
#7012 = CARTESIAN_POINT ( 'NONE',  ( 1.272929729338649674, -0.9155690868286361361, 6.310761232086846917 ) ) ;
#7013 = VECTOR ( 'NONE', #6470, 1000.000000000000114 ) ;
#7014 = ADVANCED_FACE ( 'NONE', ( #4483 ), #1545, .T. ) ;
#7015 = FACE_OUTER_BOUND ( 'NONE', #5469, .T. ) ;
#7016 = ORIENTED_EDGE ( 'NONE', *, *, #9721, .F. ) ;
#7017 = VECTOR ( 'NONE', #9361, 1000.000000000000000 ) ;
#7018 = CIRCLE ( 'NONE', #7302, 0.6500000000000000222 ) ;
#7019 = CARTESIAN_POINT ( 'NONE',  ( 1.699999999999999956, 2.299999999999999822, 7.700000000000000178 ) ) ;
#7020 =( BOUNDED_SURFACE ( )  B_SPLINE_SURFACE ( 3, 3, ( 
 ( #12211, #16371, #10633, #16281, #9232, #820, #6459, #3676, #17828, #5162, #10813, #3775, #2408, #13697, #1007, #6644, #12299, #16564, #9523, #11087, #2764, #17920, #15182, #2490, #3871, #18181, #5266, #1188, #5535, #7125, #5446, #6837, #8137, #8409, #9607, #16917, #1361, #6921, #5633, #16728, #14045, #10918, #13773, #16827, #11276, #18099, #4226, #2849, #9886, #16651, #15546, #11182, #2670, #1094, #6743, #8323, #1466, #8496, #9700, #12481, #12568, #13958 ),
 ( #12394, #3957, #1278, #4138, #15367, #7021, #18014, #11003, #9796, #14146, #4044, #5361, #15456, #12668, #17694, #15267, #2573, #8226, #13872, #17510, #11974, #8671, #9185, #5804, #15726, #1557, #7287, #4832, #13272, #6312, #672, #2061, #3030, #4494, #3110, #17586, #16232, #75, #10074, #4315, #14848, #6229, #5898, #2951, #158, #4918, #11453, #7202, #1963, #16136, #14748, #17088, #13360, #12844, #12933, #4414, #590, #262, #1640, #10148, #10480, #14238 ),
 ( #11541, #7624, #15804, #9980, #10577, #17174, #5720, #14320, #8762, #11889, #14412, #9085, #8592, #3435, #7716, #3538, #2162, #11366, #12762, #16999, #15645, #18059, #6399, #14940, #16691, #12349, #6792, #3718, #3998, #868, #10770, #2250, #2356, #17971, #8095, #1146, #13826, #15224, #16413, #16514, #9474, #12440, #11041, #13453, #5119, #17690, #9652, #1054, #960, #16324, #13551, #5401, #6507, #7902, #15137, #10964, #9566, #12254, #12166, #2449, #5317, #15321 ),
 ( #3629, #10679, #13736, #6691, #17783, #7804, #3910, #765, #9375, #9280, #2529, #8178, #12068, #5023, #15048, #8004, #2907, #14004, #12615, #4187, #14287, #8552, #12893, #16783, #7171, #2628, #9846, #1320, #6967, #15502, #4097, #9753, #5859, #15418, #2999, #2724, #7251, #8371, #18239, #6881, #8640, #8280, #11235, #16879, #2811, #13920, #212, #1519, #14087, #11505, #12722, #17135, #17045, #4460, #8452, #14199, #1419, #38, #5682, #10117, #12809, #1237 ),
 ( #11327, #16964, #4274, #122, #5770, #4369, #12526, #10030, #18139, #15689, #5487, #11129, #13073, #1691, #3416, #3078, #11585, #6030, #17216, #8721, #9065, #14629, #8901, #13341, #1787, #16118, #10190, #15956, #7431, #16038, #3257, #4629, #13156, #1944, #4538, #13250, #11952, #10289, #2040, #307, #569, #15854, #7344, #4724, #14547, #7511, #12986, #1863, #3337, #17301, #14467, #8982, #391, #14725, #4900, #15770, #6212, #7599, #654, #14366, #11869, #5946 ),
 ( #11677, #17566, #8816, #473, #3160, #6117, #17488, #4808, #7695, #6292, #10457, #11781, #17404, #10374, #4467, #3088, #5497, #15515, #9766, #1703, #11423, #11338, #8380, #5601, #5868, #11246, #12626, #7178, #3007, #1616, #16973, #16889, #4285, #4381, #8731, #15697, #8649, #1330, #12732, #10042, #7356, #18150, #14295, #131, #18251, #9857, #4197, #15605, #2820, #9943, #8563, #10125, #14378, #11140, #8464, #15429, #16795, #17056, #2919, #14015, #14103, #11514 ),
 ( #4108, #7261, #1431, #17145, #14210, #15779, #1530, #2735, #6979, #7089, #49, #5693, #12818, #5780, #12905, #227, #6223, #6304, #6042, #3176, #580, #17416, #10564, #9076, #11962, #8831, #13261, #11688, #4643, #14559, #17575, #11880, #4910, #14480, #17500, #12996, #1874, #17316, #10304, #7522, #1800, #7442, #16222, #13086, #13352, #403, #3529, #15969, #3271, #17227, #665, #318, #8911, #13167, #484, #5957, #9177, #4818, #6129, #14838, #11794, #2152 ) ),
 .UNSPECIFIED., .T., .F., .F. ) 
 B_SPLINE_SURFACE_WITH_KNOTS ( ( 4, 3, 4 ),
 ( 4, 1, 1, 1, 1, 1, 1, 1, 1, 1, 1, 1, 1, 1, 1, 1, 1, 1, 1, 1, 1, 1, 1, 1, 1, 1, 1, 1, 1, 1, 1, 1, 1, 1, 1, 1, 1, 1, 1, 1, 1, 1, 1, 1, 1, 1, 1, 1, 1, 1, 1, 1, 1, 1, 1, 1, 1, 1, 1, 4 ),
 ( 0.000000000000000000, 3.141592653589790007, 6.283185307179590673 ),
 ( 0.000000000000000000, 0.09318283294545999518, 0.1863656658909199904, 0.2795484988363799994, 0.3727313317818399807, 0.4659141647273000175, 0.5590969976727599988, 0.6522798306182200356, 0.7454626635636799614, 0.8386454965091399982, 0.9318283294545990358, 1.025011162400059961, 1.118193995345519998, 1.211376828290979812, 1.304559661236440071, 1.397742494181900108, 1.490925327127359923, 1.584108160072819960, 1.677290993018279996, 1.770473825963740033, 1.863656658909200070, 1.956839491854659885, 2.050022324800119922, 2.143205157745580181, 2.236387990691039995, 2.329570823636499810, 2.422753656581960069, 2.515936489527420328, 2.609119322472880143, 2.702302155418339957, 2.795484988363799772, 2.888667821309260031, 2.981850654254720290, 3.075033487200180105, 3.168216320145639919, 3.261399153091099734, 3.354581986036559993, 3.447764818982019808, 3.540947651927480067, 3.634130484872939881, 3.727313317818400140, 3.820496150763859955, 3.913678983709319770, 4.006861816654780029, 4.100044649600239843, 4.193227482545699658, 4.286410315491160361, 4.379593148436620176, 4.472775981382079991, 4.565958814327539805, 4.659141647272999620, 4.752324480218450553, 4.845507313163910368, 4.938690146109370183, 5.031872979054829997, 5.125055812000289812, 5.218238644945749627, 5.311421477891210330, 5.404604310836670145, 5.497787143782139729 ),
 .UNSPECIFIED. ) 
 GEOMETRIC_REPRESENTATION_ITEM ( )  RATIONAL_B_SPLINE_SURFACE ( (
 ( 1.000000000000000000, 1.000000000000000000, 1.000000000000000000, 1.000000000000000000, 1.000000000000000000, 1.000000000000000000, 1.000000000000000000, 1.000000000000000000, 1.000000000000000000, 1.000000000000000000, 1.000000000000000000, 1.000000000000000000, 1.000000000000000000, 1.000000000000000000, 1.000000000000000000, 1.000000000000000000, 1.000000000000000000, 1.000000000000000000, 1.000000000000000000, 1.000000000000000000, 1.000000000000000000, 1.000000000000000000, 1.000000000000000000, 1.000000000000000000, 1.000000000000000000, 1.000000000000000000, 1.000000000000000000, 1.000000000000000000, 1.000000000000000000, 1.000000000000000000, 1.000000000000000000, 1.000000000000000000, 1.000000000000000000, 1.000000000000000000, 1.000000000000000000, 1.000000000000000000, 1.000000000000000000, 1.000000000000000000, 1.000000000000000000, 1.000000000000000000, 1.000000000000000000, 1.000000000000000000, 1.000000000000000000, 1.000000000000000000, 1.000000000000000000, 1.000000000000000000, 1.000000000000000000, 1.000000000000000000, 1.000000000000000000, 1.000000000000000000, 1.000000000000000000, 1.000000000000000000, 1.000000000000000000, 1.000000000000000000, 1.000000000000000000, 1.000000000000000000, 1.000000000000000000, 1.000000000000000000, 1.000000000000000000, 1.000000000000000000, 1.000000000000000000, 1.000000000000000000),
 ( 0.3333333333333329818, 0.3333333333333329818, 0.3333333333333329818, 0.3333333333333329818, 0.3333333333333329818, 0.3333333333333329818, 0.3333333333333329818, 0.3333333333333329818, 0.3333333333333329818, 0.3333333333333329818, 0.3333333333333329818, 0.3333333333333329818, 0.3333333333333329818, 0.3333333333333329818, 0.3333333333333329818, 0.3333333333333329818, 0.3333333333333329818, 0.3333333333333329818, 0.3333333333333329818, 0.3333333333333329818, 0.3333333333333329818, 0.3333333333333329818, 0.3333333333333329818, 0.3333333333333329818, 0.3333333333333329818, 0.3333333333333329818, 0.3333333333333329818, 0.3333333333333329818, 0.3333333333333329818, 0.3333333333333329818, 0.3333333333333329818, 0.3333333333333329818, 0.3333333333333329818, 0.3333333333333329818, 0.3333333333333329818, 0.3333333333333329818, 0.3333333333333329818, 0.3333333333333329818, 0.3333333333333329818, 0.3333333333333329818, 0.3333333333333329818, 0.3333333333333329818, 0.3333333333333329818, 0.3333333333333329818, 0.3333333333333329818, 0.3333333333333329818, 0.3333333333333329818, 0.3333333333333329818, 0.3333333333333329818, 0.3333333333333329818, 0.3333333333333329818, 0.3333333333333329818, 0.3333333333333329818, 0.3333333333333329818, 0.3333333333333329818, 0.3333333333333329818, 0.3333333333333329818, 0.3333333333333329818, 0.3333333333333329818, 0.3333333333333329818, 0.3333333333333329818, 0.3333333333333329818),
 ( 0.3333333333333329818, 0.3333333333333329818, 0.3333333333333329818, 0.3333333333333329818, 0.3333333333333329818, 0.3333333333333329818, 0.3333333333333329818, 0.3333333333333329818, 0.3333333333333329818, 0.3333333333333329818, 0.3333333333333329818, 0.3333333333333329818, 0.3333333333333329818, 0.3333333333333329818, 0.3333333333333329818, 0.3333333333333329818, 0.3333333333333329818, 0.3333333333333329818, 0.3333333333333329818, 0.3333333333333329818, 0.3333333333333329818, 0.3333333333333329818, 0.3333333333333329818, 0.3333333333333329818, 0.3333333333333329818, 0.3333333333333329818, 0.3333333333333329818, 0.3333333333333329818, 0.3333333333333329818, 0.3333333333333329818, 0.3333333333333329818, 0.3333333333333329818, 0.3333333333333329818, 0.3333333333333329818, 0.3333333333333329818, 0.3333333333333329818, 0.3333333333333329818, 0.3333333333333329818, 0.3333333333333329818, 0.3333333333333329818, 0.3333333333333329818, 0.3333333333333329818, 0.3333333333333329818, 0.3333333333333329818, 0.3333333333333329818, 0.3333333333333329818, 0.3333333333333329818, 0.3333333333333329818, 0.3333333333333329818, 0.3333333333333329818, 0.3333333333333329818, 0.3333333333333329818, 0.3333333333333329818, 0.3333333333333329818, 0.3333333333333329818, 0.3333333333333329818, 0.3333333333333329818, 0.3333333333333329818, 0.3333333333333329818, 0.3333333333333329818, 0.3333333333333329818, 0.3333333333333329818),
 ( 1.000000000000000000, 1.000000000000000000, 1.000000000000000000, 1.000000000000000000, 1.000000000000000000, 1.000000000000000000, 1.000000000000000000, 1.000000000000000000, 1.000000000000000000, 1.000000000000000000, 1.000000000000000000, 1.000000000000000000, 1.000000000000000000, 1.000000000000000000, 1.000000000000000000, 1.000000000000000000, 1.000000000000000000, 1.000000000000000000, 1.000000000000000000, 1.000000000000000000, 1.000000000000000000, 1.000000000000000000, 1.000000000000000000, 1.000000000000000000, 1.000000000000000000, 1.000000000000000000, 1.000000000000000000, 1.000000000000000000, 1.000000000000000000, 1.000000000000000000, 1.000000000000000000, 1.000000000000000000, 1.000000000000000000, 1.000000000000000000, 1.000000000000000000, 1.000000000000000000, 1.000000000000000000, 1.000000000000000000, 1.000000000000000000, 1.000000000000000000, 1.000000000000000000, 1.000000000000000000, 1.000000000000000000, 1.000000000000000000, 1.000000000000000000, 1.000000000000000000, 1.000000000000000000, 1.000000000000000000, 1.000000000000000000, 1.000000000000000000, 1.000000000000000000, 1.000000000000000000, 1.000000000000000000, 1.000000000000000000, 1.000000000000000000, 1.000000000000000000, 1.000000000000000000, 1.000000000000000000, 1.000000000000000000, 1.000000000000000000, 1.000000000000000000, 1.000000000000000000),
 ( 0.3333333333333329818, 0.3333333333333329818, 0.3333333333333329818, 0.3333333333333329818, 0.3333333333333329818, 0.3333333333333329818, 0.3333333333333329818, 0.3333333333333329818, 0.3333333333333329818, 0.3333333333333329818, 0.3333333333333329818, 0.3333333333333329818, 0.3333333333333329818, 0.3333333333333329818, 0.3333333333333329818, 0.3333333333333329818, 0.3333333333333329818, 0.3333333333333329818, 0.3333333333333329818, 0.3333333333333329818, 0.3333333333333329818, 0.3333333333333329818, 0.3333333333333329818, 0.3333333333333329818, 0.3333333333333329818, 0.3333333333333329818, 0.3333333333333329818, 0.3333333333333329818, 0.3333333333333329818, 0.3333333333333329818, 0.3333333333333329818, 0.3333333333333329818, 0.3333333333333329818, 0.3333333333333329818, 0.3333333333333329818, 0.3333333333333329818, 0.3333333333333329818, 0.3333333333333329818, 0.3333333333333329818, 0.3333333333333329818, 0.3333333333333329818, 0.3333333333333329818, 0.3333333333333329818, 0.3333333333333329818, 0.3333333333333329818, 0.3333333333333329818, 0.3333333333333329818, 0.3333333333333329818, 0.3333333333333329818, 0.3333333333333329818, 0.3333333333333329818, 0.3333333333333329818, 0.3333333333333329818, 0.3333333333333329818, 0.3333333333333329818, 0.3333333333333329818, 0.3333333333333329818, 0.3333333333333329818, 0.3333333333333329818, 0.3333333333333329818, 0.3333333333333329818, 0.3333333333333329818),
 ( 0.3333333333333329818, 0.3333333333333329818, 0.3333333333333329818, 0.3333333333333329818, 0.3333333333333329818, 0.3333333333333329818, 0.3333333333333329818, 0.3333333333333329818, 0.3333333333333329818, 0.3333333333333329818, 0.3333333333333329818, 0.3333333333333329818, 0.3333333333333329818, 0.3333333333333329818, 0.3333333333333329818, 0.3333333333333329818, 0.3333333333333329818, 0.3333333333333329818, 0.3333333333333329818, 0.3333333333333329818, 0.3333333333333329818, 0.3333333333333329818, 0.3333333333333329818, 0.3333333333333329818, 0.3333333333333329818, 0.3333333333333329818, 0.3333333333333329818, 0.3333333333333329818, 0.3333333333333329818, 0.3333333333333329818, 0.3333333333333329818, 0.3333333333333329818, 0.3333333333333329818, 0.3333333333333329818, 0.3333333333333329818, 0.3333333333333329818, 0.3333333333333329818, 0.3333333333333329818, 0.3333333333333329818, 0.3333333333333329818, 0.3333333333333329818, 0.3333333333333329818, 0.3333333333333329818, 0.3333333333333329818, 0.3333333333333329818, 0.3333333333333329818, 0.3333333333333329818, 0.3333333333333329818, 0.3333333333333329818, 0.3333333333333329818, 0.3333333333333329818, 0.3333333333333329818, 0.3333333333333329818, 0.3333333333333329818, 0.3333333333333329818, 0.3333333333333329818, 0.3333333333333329818, 0.3333333333333329818, 0.3333333333333329818, 0.3333333333333329818, 0.3333333333333329818, 0.3333333333333329818),
 ( 1.000000000000000000, 1.000000000000000000, 1.000000000000000000, 1.000000000000000000, 1.000000000000000000, 1.000000000000000000, 1.000000000000000000, 1.000000000000000000, 1.000000000000000000, 1.000000000000000000, 1.000000000000000000, 1.000000000000000000, 1.000000000000000000, 1.000000000000000000, 1.000000000000000000, 1.000000000000000000, 1.000000000000000000, 1.000000000000000000, 1.000000000000000000, 1.000000000000000000, 1.000000000000000000, 1.000000000000000000, 1.000000000000000000, 1.000000000000000000, 1.000000000000000000, 1.000000000000000000, 1.000000000000000000, 1.000000000000000000, 1.000000000000000000, 1.000000000000000000, 1.000000000000000000, 1.000000000000000000, 1.000000000000000000, 1.000000000000000000, 1.000000000000000000, 1.000000000000000000, 1.000000000000000000, 1.000000000000000000, 1.000000000000000000, 1.000000000000000000, 1.000000000000000000, 1.000000000000000000, 1.000000000000000000, 1.000000000000000000, 1.000000000000000000, 1.000000000000000000, 1.000000000000000000, 1.000000000000000000, 1.000000000000000000, 1.000000000000000000, 1.000000000000000000, 1.000000000000000000, 1.000000000000000000, 1.000000000000000000, 1.000000000000000000, 1.000000000000000000, 1.000000000000000000, 1.000000000000000000, 1.000000000000000000, 1.000000000000000000, 1.000000000000000000, 1.000000000000000000) ) ) 
 REPRESENTATION_ITEM ( '' )  SURFACE ( )  );
#7021 = CARTESIAN_POINT ( 'NONE',  ( 0.9664230948141925293, -0.3177966101694921219, 2.228384861502251457 ) ) ;
#7022 = CARTESIAN_POINT ( 'NONE',  ( 2.169623098572349917, -2.658349832090280529, 5.611855963200990338 ) ) ;
#7023 = LINE ( 'NONE', #10076, #13101 ) ;
#7024 = CARTESIAN_POINT ( 'NONE',  ( -2.500000000000000000, 1.071484571201660082E-16, -4.257195078628519890E-16 ) ) ;
#7025 = CARTESIAN_POINT ( 'NONE',  ( 2.171642826483958899, -5.104237288135595740, 6.225392547715717484 ) ) ;
#7026 = EDGE_LOOP ( 'NONE', ( #15601, #3384, #6441, #10897 ) ) ;
#7027 = AXIS2_PLACEMENT_3D ( 'NONE', #54, #18073, #13936 ) ;
#7028 = VECTOR ( 'NONE', #15557, 1000.000000000000000 ) ;
#7029 = ORIENTED_EDGE ( 'NONE', *, *, #5421, .T. ) ;
#7030 = CARTESIAN_POINT ( 'NONE',  ( -2.116444151961479392, -5.246610169491528808, 3.670839500609360151 ) ) ;
#7031 = PLANE ( 'NONE',  #4972 ) ;
#7032 = CARTESIAN_POINT ( 'NONE',  ( -1.899999999999999911, 0.5999999999999999778, 6.599999999999999645 ) ) ;
#7033 = ADVANCED_FACE ( 'NONE', ( #15535 ), #9965, .T. ) ;
#7034 = ORIENTED_EDGE ( 'NONE', *, *, #18192, .T. ) ;
#7035 = AXIS2_PLACEMENT_3D ( 'NONE', #2524, #13816, #1228 ) ;
#7036 = AXIS2_PLACEMENT_3D ( 'NONE', #8628, #7158, #14271 ) ;
#7037 = CARTESIAN_POINT ( 'NONE',  ( -2.352190863465239978, -4.917313796054239461, 4.622903765856379188 ) ) ;
#7038 = VECTOR ( 'NONE', #1620, 1000.000000000000000 ) ;
#7039 = DIRECTION ( 'NONE',  ( 1.110223024625159992E-16, 2.220446049250309876E-16, -1.000000000000000000 ) ) ;
#7040 = CARTESIAN_POINT ( 'NONE',  ( 1.534924416212170017, -5.333856471232000018, 2.911460733964629899 ) ) ;
#7041 = DIRECTION ( 'NONE',  ( 0.000000000000000000, -1.000000000000000000, 0.000000000000000000 ) ) ;
#7042 = CARTESIAN_POINT ( 'NONE',  ( 2.352190863465239978, -0.6826862039457530784, 4.622903765856330338 ) ) ;
#7043 = CARTESIAN_POINT ( 'NONE',  ( -2.500000000000000000, 2.799999999999999822, 0.5999999999999999778 ) ) ;
#7044 = AXIS2_PLACEMENT_3D ( 'NONE', #7101, #13939, #3931 ) ;
#7045 = CARTESIAN_POINT ( 'NONE',  ( 0.3949552299394610277, -3.776187669928119828, 2.379923265530350385 ) ) ;
#7046 = VECTOR ( 'NONE', #10911, 1000.000000000000000 ) ;
#7047 = DIRECTION ( 'NONE',  ( -1.000000000000000000, 0.000000000000000000, 6.123233995736769734E-17 ) ) ;
#7048 = CARTESIAN_POINT ( 'NONE',  ( -1.454969160281959661, -3.147403886144331420, 6.148435909958226198 ) ) ;
#7049 = EDGE_CURVE ( 'NONE', #18253, #8865, #7018, .T. ) ;
#7050 = DIRECTION ( 'NONE',  ( -1.930822651522009842E-16, -1.000000000000000000, -1.268826313857319964E-16 ) ) ;
#7051 = CARTESIAN_POINT ( 'NONE',  ( 1.428515267734870031, -0.3311440677966109858, 2.829745655876919841 ) ) ;
#7052 = VECTOR ( 'NONE', #10399, 1000.000000000000000 ) ;
#7053 = EDGE_LOOP ( 'NONE', ( #12017, #10171, #11903, #14598 ) ) ;
#7054 = CARTESIAN_POINT ( 'NONE',  ( -0.8244235255442939891, -0.5829339996946389935, 2.492493020344019872 ) ) ;
#7055 = ORIENTED_EDGE ( 'NONE', *, *, #6875, .T. ) ;
#7056 = VECTOR ( 'NONE', #17182, 1000.000000000000000 ) ;
#7057 = DIRECTION ( 'NONE',  ( 6.661338147750940229E-16, -1.710569414459004727E-47, 1.000000000000000000 ) ) ;
#7058 = ORIENTED_EDGE ( 'NONE', *, *, #14259, .F. ) ;
#7059 = DIRECTION ( 'NONE',  ( -0.000000000000000000, 1.000000000000000000, 0.000000000000000000 ) ) ;
#7060 = LINE ( 'NONE', #14344, #1443 ) ;
#7061 = ADVANCED_FACE ( 'NONE', ( #7003 ), #14578, .T. ) ;
#7062 = VECTOR ( 'NONE', #8389, 1000.000000000000000 ) ;
#7063 = EDGE_LOOP ( 'NONE', ( #14631, #2248, #7185, #12534 ) ) ;
#7064 = VECTOR ( 'NONE', #12189, 1000.000000000000000 ) ;
#7065 = CARTESIAN_POINT ( 'NONE',  ( -0.3265524029357583236, -5.157627118644064979, 6.726831181542982208 ) ) ;
#7066 = CARTESIAN_POINT ( 'NONE',  ( 1.800000000000000044, 0.5999999999999999778, 1.600000000000000089 ) ) ;
#7067 = PLANE ( 'NONE',  #17928 ) ;
#7068 = VECTOR ( 'NONE', #12210, 1000.000000000000000 ) ;
#7069 = VECTOR ( 'NONE', #8969, 1000.000000000000000 ) ;
#7070 = DIRECTION ( 'NONE',  ( 0.000000000000000000, -1.000000000000000000, -1.332267629550190018E-15 ) ) ;
#7071 = DIRECTION ( 'NONE',  ( 1.306144734853129823E-16, -1.000000000000000000, -1.306144734853129823E-16 ) ) ;
#7072 = CARTESIAN_POINT ( 'NONE',  ( 1.074829861819710075, -2.285737219477669946, 2.606322265575589991 ) ) ;
#7073 = CARTESIAN_POINT ( 'NONE',  ( 1.385380178477290558, -3.617010528270069525, 3.184868453331423765 ) ) ;
#7074 = CARTESIAN_POINT ( 'NONE',  ( 1.965557623688110933, -0.08898305084745804228, 5.292675575926325315 ) ) ;
#7075 = VECTOR ( 'NONE', #6600, 1000.000000000000000 ) ;
#7076 = LINE ( 'NONE', #18235, #17348 ) ;
#7077 = DIRECTION ( 'NONE',  ( 1.110223024625159992E-16, 0.000000000000000000, -1.000000000000000000 ) ) ;
#7078 = ORIENTED_EDGE ( 'NONE', *, *, #5217, .F. ) ;
#7079 = CARTESIAN_POINT ( 'NONE',  ( -2.255259958075430227, -1.703530012270459970, 5.372717034856060003 ) ) ;
#7080 = ORIENTED_EDGE ( 'NONE', *, *, #14124, .T. ) ;
#7081 = AXIS2_PLACEMENT_3D ( 'NONE', #2076, #17889, #7730 ) ;
#7082 = EDGE_LOOP ( 'NONE', ( #7194, #11633, #4834, #12841 ) ) ;
#7083 = CARTESIAN_POINT ( 'NONE',  ( -1.866416942370659804, -1.637506023765569640, 3.266391446483499106 ) ) ;
#7084 = CARTESIAN_POINT ( 'NONE',  ( 0.000000000000000000, 0.000000000000000000, 0.000000000000000000 ) ) ;
#7085 = CARTESIAN_POINT ( 'NONE',  ( 0.5609751937345880402, -5.439830508474575943, 7.293870047334757523 ) ) ;
#7086 = ORIENTED_EDGE ( 'NONE', *, *, #3920, .T. ) ;
#7087 =( GEOMETRIC_REPRESENTATION_CONTEXT ( 3 ) GLOBAL_UNCERTAINTY_ASSIGNED_CONTEXT ( ( #12703 ) ) GLOBAL_UNIT_ASSIGNED_CONTEXT ( ( #9480, #14011, #6696 ) ) REPRESENTATION_CONTEXT ( 'NONE', 'WORKASPACE' ) );
#7088 = CARTESIAN_POINT ( 'NONE',  ( 2.053221424930760097, -0.8651516338920849369, 3.549770689668250157 ) ) ;
#7089 = CARTESIAN_POINT ( 'NONE',  ( 1.596341326794969984, -0.3355932203389830337, 2.970780074643809776 ) ) ;
#7090 = ADVANCED_FACE ( 'NONE', ( #5215 ), #12103, .T. ) ;
#7091 = ORIENTED_EDGE ( 'NONE', *, *, #14840, .F. ) ;
#7092 = DIRECTION ( 'NONE',  ( 3.700743415417190309E-15, 1.480297366166879989E-15, -1.000000000000000000 ) ) ;
#7093 = CARTESIAN_POINT ( 'NONE',  ( -0.5500000000000000444, 6.450000000000000178, 3.600000000000000089 ) ) ;
#7094 = FACE_OUTER_BOUND ( 'NONE', #4831, .T. ) ;
#7095 = CIRCLE ( 'NONE', #5899, 0.3999999999999999667 ) ;
#7096 = CARTESIAN_POINT ( 'NONE',  ( -1.698651900122509995, -3.193980462720909408, 5.853032334688971439 ) ) ;
#7097 = CARTESIAN_POINT ( 'NONE',  ( -1.800000000000000044, 0.5999999999999999778, 7.599999999999999645 ) ) ;
#7098 = CARTESIAN_POINT ( 'NONE',  ( 1.407651048079441525, -0.3266949152542383272, 2.450250343405061759 ) ) ;
#7099 = ORIENTED_EDGE ( 'NONE', *, *, #3920, .F. ) ;
#7100 = CARTESIAN_POINT ( 'NONE',  ( -2.500000000000000000, 2.799999999999999822, 1.600000000000000089 ) ) ;
#7101 = CARTESIAN_POINT ( 'NONE',  ( 1.699999999999999956, 9.299999999999998934, 7.599999999999999645 ) ) ;
#7102 = CARTESIAN_POINT ( 'NONE',  ( -0.05465110135555984600, -0.4512711864406789841, 6.752241303418941243 ) ) ;
#7103 = PRODUCT_DEFINITION_FORMATION_WITH_SPECIFIED_SOURCE ( 'ANY', '', #9637, .NOT_KNOWN. ) ;
#7104 = EDGE_CURVE ( 'NONE', #8925, #4902, #1352, .T. ) ;
#7105 = EDGE_LOOP ( 'NONE', ( #15868, #14343, #6598, #420 ) ) ;
#7106 = CARTESIAN_POINT ( 'NONE',  ( -0.5027094486773525661, -4.952022267818764867, 2.083735201298030137 ) ) ;
#7107 = CARTESIAN_POINT ( 'NONE',  ( 1.943632316591230147, -5.346398305084740343, 3.373048379518159834 ) ) ;
#7108 = VERTEX_POINT ( 'NONE', #14132 ) ;
#7109 = CARTESIAN_POINT ( 'NONE',  ( 0.4360591020457930123, -0.008898305084746038762, 2.387347919655840034 ) ) ;
#7110 = AXIS2_PLACEMENT_3D ( 'NONE', #15926, #17194, #17467 ) ;
#7111 = SPHERICAL_SURFACE ( 'NONE', #14104, 1.100000000000000089 ) ;
#7112 = ORIENTED_EDGE ( 'NONE', *, *, #4777, .F. ) ;
#7113 = LINE ( 'NONE', #17165, #12343 ) ;
#7114 = CARTESIAN_POINT ( 'NONE',  ( -1.991984774470509922, -1.614217735477279980, 3.446707398186049875 ) ) ;
#7115 = LINE ( 'NONE', #2760, #1712 ) ;
#7116 = CARTESIAN_POINT ( 'NONE',  ( 1.549925137359331462, -0.8689925102520592581, 6.046340934239826659 ) ) ;
#7117 = APPLICATION_CONTEXT ( 'automotive_design' ) ;
#7118 = CARTESIAN_POINT ( 'NONE',  ( -1.699999999999999956, 2.299999999999999822, 7.599999999999999645 ) ) ;
#7119 = EDGE_CURVE ( 'NONE', #17218, #10817, #5796, .T. ) ;
#7120 = EDGE_LOOP ( 'NONE', ( #3241, #15298, #10416, #1129 ) ) ;
#7121 = AXIS2_PLACEMENT_3D ( 'NONE', #5989, #17354, #6251 ) ;
#7122 = PRODUCT_DEFINITION ( 'UNKNOWN', '', #1478, #1396 ) ;
#7123 = EDGE_CURVE ( 'NONE', #4205, #14294, #5523, .T. ) ;
#7124 = CARTESIAN_POINT ( 'NONE',  ( 1.710144332342950158, -5.052039382343889606, 2.989855667657050020 ) ) ;
#7125 = CARTESIAN_POINT ( 'NONE',  ( 1.194742379459969861, -0.4245762711864409789, 6.727584234649759409 ) ) ;
#7126 = EDGE_CURVE ( 'NONE', #12165, #10292, #12657, .T. ) ;
#7127 = CARTESIAN_POINT ( 'NONE',  ( 2.075124426334590044, -2.681638120378570189, 5.810227140144509583 ) ) ;
#7128 = CARTESIAN_POINT ( 'NONE',  ( 1.899999999999999911, 1.010812223616570040E-16, 4.000000000000000000 ) ) ;
#7129 = EDGE_CURVE ( 'NONE', #6319, #5435, #9367, .T. ) ;
#7130 = CARTESIAN_POINT ( 'NONE',  ( -1.899999999999999911, 11.15000000000000036, 1.600000000000000089 ) ) ;
#7131 = CARTESIAN_POINT ( 'NONE',  ( 2.431060148753489081, -5.055296610169490279, 3.635668498923322112 ) ) ;
#7132 = ORIENTED_EDGE ( 'NONE', *, *, #17696, .F. ) ;
#7133 = ORIENTED_EDGE ( 'NONE', *, *, #6563, .F. ) ;
#7134 = DIRECTION ( 'NONE',  ( -4.810966440042350793E-15, 0.000000000000000000, -1.000000000000000000 ) ) ;
#7135 = CARTESIAN_POINT ( 'NONE',  ( 0.5500000000000000444, 7.799999999999999822, 1.600000000000000089 ) ) ;
#7136 = ORIENTED_EDGE ( 'NONE', *, *, #34, .T. ) ;
#7137 = VECTOR ( 'NONE', #14051, 1000.000000000000000 ) ;
#7138 = CARTESIAN_POINT ( 'NONE',  ( 0.3162622016569809347, -1.354205687946139491, 7.334974746141788238 ) ) ;
#7139 = CARTESIAN_POINT ( 'NONE',  ( 0.5803392541454069908, -5.011796459788059543, 2.403119802722879950 ) ) ;
#7140 = DIRECTION ( 'NONE',  ( 0.000000000000000000, -1.000000000000000000, 0.000000000000000000 ) ) ;
#7141 = CARTESIAN_POINT ( 'NONE',  ( 1.914021115237030113, -0.8457042219637709302, 6.069404563272200015 ) ) ;
#7142 = CARTESIAN_POINT ( 'NONE',  ( 1.550000000000000044, -5.599999999999999645, 5.100000000000000533 ) ) ;
#7143 = EDGE_CURVE ( 'NONE', #15958, #1298, #67, .T. ) ;
#7144 = CARTESIAN_POINT ( 'NONE',  ( 2.260890494820590124, -4.055647129387580208, 4.046455925041149371 ) ) ;
#7145 = DIRECTION ( 'NONE',  ( 1.000000000000000000, 0.000000000000000000, 0.000000000000000000 ) ) ;
#7146 = CARTESIAN_POINT ( 'NONE',  ( -0.6050872056802790722, -3.659746228486683073, 2.738171435586149727 ) ) ;
#7147 = EDGE_CURVE ( 'NONE', #12988, #12167, #5533, .T. ) ;
#7148 = DIRECTION ( 'NONE',  ( 0.000000000000000000, 0.000000000000000000, 1.000000000000000000 ) ) ;
#7149 = VECTOR ( 'NONE', #16236, 1000.000000000000000 ) ;
#7150 = VERTEX_POINT ( 'NONE', #16909 ) ;
#7151 = CARTESIAN_POINT ( 'NONE',  ( -0.4617942143426889690, -0.5906145504024210569, 2.383143958488499692 ) ) ;
#7152 = ORIENTED_EDGE ( 'NONE', *, *, #13307, .T. ) ;
#7153 = CARTESIAN_POINT ( 'NONE',  ( 1.250000000000000000, 6.144112549695430303, 5.100000000000000533 ) ) ;
#7154 = ORIENTED_EDGE ( 'NONE', *, *, #16095, .T. ) ;
#7155 = CARTESIAN_POINT ( 'NONE',  ( 1.399999999999999911, 5.799999999999999822, 8.300000000000000711 ) ) ;
#7156 = ORIENTED_EDGE ( 'NONE', *, *, #12310, .T. ) ;
#7157 = CARTESIAN_POINT ( 'NONE',  ( 1.940327948426050941, -5.090889830508485758, 5.370677689277660427 ) ) ;
#7158 = DIRECTION ( 'NONE',  ( -4.794417550286630491E-31, 1.000000000000000000, 1.774290917998389804E-45 ) ) ;
#7159 = CARTESIAN_POINT ( 'NONE',  ( -0.5291502622129179434, 0.1000000000000000056, 7.700000000000000178 ) ) ;
#7160 = DIRECTION ( 'NONE',  ( 1.000000000000000000, 0.000000000000000000, 1.850371707708589879E-16 ) ) ;
#7161 = CARTESIAN_POINT ( 'NONE',  ( -1.229686204202100175, -5.164643153926309793, 2.674737924334550154 ) ) ;
#7162 = CARTESIAN_POINT ( 'NONE',  ( -1.875000000000000000, 12.00000000000000000, 7.700000000000000178 ) ) ;
#7163 = DIRECTION ( 'NONE',  ( 2.960594732333750117E-16, -1.000000000000000000, 0.000000000000000000 ) ) ;
#7164 = CARTESIAN_POINT ( 'NONE',  ( 2.245209214543399945, -2.635061543801989981, 5.405536158119010004 ) ) ;
#7165 = CARTESIAN_POINT ( 'NONE',  ( 0.9123513484651973870, -3.547145663405211646, 2.860838000723751051 ) ) ;
#7166 = CARTESIAN_POINT ( 'NONE',  ( 1.725722849164588624, -0.1023305084745770588, 5.812007984777676661 ) ) ;
#7167 = EDGE_CURVE ( 'NONE', #7523, #8572, #16816, .T. ) ;
#7168 = CARTESIAN_POINT ( 'NONE',  ( 0.1749999999999999889, 4.299999999999999822, 0.5999999999999999778 ) ) ;
#7169 = CYLINDRICAL_SURFACE ( 'NONE', #8567, 0.2499999999999996669 ) ;
#7170 = VERTEX_POINT ( 'NONE', #8750 ) ;
#7171 = CARTESIAN_POINT ( 'NONE',  ( 1.978267656359410154, -0.1023305084745769894, 5.974740860598790171 ) ) ;
#7172 = CARTESIAN_POINT ( 'NONE',  ( -2.353343516942199898, -1.773394877135329839, 4.722803042560189901 ) ) ;
#7173 = ORIENTED_EDGE ( 'NONE', *, *, #874, .F. ) ;
#7174 = VERTEX_POINT ( 'NONE', #17077 ) ;
#7175 = CARTESIAN_POINT ( 'NONE',  ( 1.332058588847409686, -2.499172690432239108, 6.640197310420187904 ) ) ;
#7176 = CARTESIAN_POINT ( 'NONE',  ( -2.614198783383141045, -5.533262711864405325, 4.243032045539295360 ) ) ;
#7177 = EDGE_LOOP ( 'NONE', ( #2044, #3437, #15737, #1365 ) ) ;
#7178 = CARTESIAN_POINT ( 'NONE',  ( 1.351903350398191206, -0.4156779661016956062, 6.245004350000406212 ) ) ;
#7179 = EDGE_LOOP ( 'NONE', ( #14648, #17228, #14420, #5795 ) ) ;
#7180 = AXIS2_PLACEMENT_3D ( 'NONE', #14872, #3652, #3999 ) ;
#7181 = LINE ( 'NONE', #7445, #15581 ) ;
#7182 = LINE ( 'NONE', #8652, #12641 ) ;
#7183 = CARTESIAN_POINT ( 'NONE',  ( -0.08304008649493913041, -2.961097579838030569, 6.751342532748503267 ) ) ;
#7184 = CARTESIAN_POINT ( 'NONE',  ( 1.925836318347889931, -0.4112288135593234473, 6.525927015348126581 ) ) ;
#7185 = ORIENTED_EDGE ( 'NONE', *, *, #1374, .F. ) ;
#7186 = CARTESIAN_POINT ( 'NONE',  ( -0.009452110982656868748, -5.299807955295460005, 2.350000000000000089 ) ) ;
#7187 = CARTESIAN_POINT ( 'NONE',  ( -1.800000000000000044, 11.29999999999999893, 7.649999999999999467 ) ) ;
#7188 = EDGE_LOOP ( 'NONE', ( #13030, #6562, #12055, #6381, #3038, #12153, #8984, #5867, #11753, #12573, #3098, #18277, #12033, #9281, #13708, #14050, #1036, #16446 ) ) ;
#7189 = LINE ( 'NONE', #10133, #12433 ) ;
#7190 = CARTESIAN_POINT ( 'NONE',  ( -1.526871680339578541, -5.559957627118640389, 3.327650196883449762 ) ) ;
#7191 = AXIS2_PLACEMENT_3D ( 'NONE', #4116, #18158, #4017 ) ;
#7192 = DIRECTION ( 'NONE',  ( 0.000000000000000000, 0.000000000000000000, -1.000000000000000000 ) ) ;
#7193 = CARTESIAN_POINT ( 'NONE',  ( 0.7093417302541469294, -5.435381355932199732, 6.943956659919690466 ) ) ;
#7194 = ORIENTED_EDGE ( 'NONE', *, *, #8374, .T. ) ;
#7195 = CARTESIAN_POINT ( 'NONE',  ( -1.408343819019460219E-16, 2.299999999999999822, 5.100000000000000533 ) ) ;
#7196 = CARTESIAN_POINT ( 'NONE',  ( -2.343457872958619959, -1.451199717459269900, 4.916681529328609912 ) ) ;
#7197 = LINE ( 'NONE', #8753, #5511 ) ;
#7198 = CARTESIAN_POINT ( 'NONE',  ( -0.2993653819235400082, -2.685478996738538626, 6.731079075450757898 ) ) ;
#7199 = CARTESIAN_POINT ( 'NONE',  ( 0.3042893218813449985, 3.050000000000000266, 2.170710678118660031 ) ) ;
#7200 = VERTEX_POINT ( 'NONE', #12835 ) ;
#7201 = CARTESIAN_POINT ( 'NONE',  ( 0.5637478356992829953, -0.6606104644819250638, 2.398845082743519708 ) ) ;
#7202 = CARTESIAN_POINT ( 'NONE',  ( -2.416676968769249090, -0.5046610169491535514, 5.796598111919839980 ) ) ;
#7203 = CARTESIAN_POINT ( 'NONE',  ( 1.397172971746949877, -3.892629111369559691, 2.806153814454899642 ) ) ;
#7204 = LINE ( 'NONE', #12846, #14573 ) ;
#7205 = CARTESIAN_POINT ( 'NONE',  ( 0.5000000000000000000, 5.762741699796949391, 5.100000000000000533 ) ) ;
#7206 = CARTESIAN_POINT ( 'NONE',  ( 1.811729841638690219, -5.041949152542369639, 3.197954009834290012 ) ) ;
#7207 = ORIENTED_EDGE ( 'NONE', *, *, #14655, .F. ) ;
#7208 = VERTEX_POINT ( 'NONE', #11267 ) ;
#7209 = CARTESIAN_POINT ( 'NONE',  ( 1.899999999999999911, 2.799999999999999822, 0.6099999999999999867 ) ) ;
#7210 = LINE ( 'NONE', #4147, #4663 ) ;
#7211 = ORIENTED_EDGE ( 'NONE', *, *, #8312, .T. ) ;
#7212 = CARTESIAN_POINT ( 'NONE',  ( -1.820241257191459905, -5.080331814072259533, 3.208199930689799917 ) ) ;
#7213 = EDGE_CURVE ( 'NONE', #14122, #15958, #11532, .T. ) ;
#7214 = CARTESIAN_POINT ( 'NONE',  ( 1.440522616026430391, -0.7952867690272208412, 3.241384813161591438 ) ) ;
#7215 = CARTESIAN_POINT ( 'NONE',  ( 0.03000000000000110217, 11.40000000000000036, 7.649999999999999467 ) ) ;
#7216 = EDGE_CURVE ( 'NONE', #16761, #6275, #15449, .T. ) ;
#7217 = CARTESIAN_POINT ( 'NONE',  ( -0.4000000000000000222, -1.399999999999999911, 5.100000000000000533 ) ) ;
#7218 = CARTESIAN_POINT ( 'NONE',  ( -2.352760675243210198, -3.034803321062869763, 4.757121734156080528 ) ) ;
#7219 = EDGE_CURVE ( 'NONE', #13449, #11068, #14037, .T. ) ;
#7220 = DIRECTION ( 'NONE',  ( -2.220446049250309876E-16, -1.000000000000000000, 1.110223024625159992E-16 ) ) ;
#7221 = CARTESIAN_POINT ( 'NONE',  ( 1.397172971746949877, -3.892629111369559691, 2.806153814454899642 ) ) ;
#7222 = DIRECTION ( 'NONE',  ( 1.000000000000000000, 0.000000000000000000, 0.000000000000000000 ) ) ;
#7223 = CARTESIAN_POINT ( 'NONE',  ( 1.974086094277279768, -4.195376859117311064, 5.263813741415705572 ) ) ;
#7224 = DIRECTION ( 'NONE',  ( 1.586032892321649771E-16, -1.000000000000000000, 0.000000000000000000 ) ) ;
#7225 = ORIENTED_EDGE ( 'NONE', *, *, #12132, .T. ) ;
#7226 = LINE ( 'NONE', #8527, #585 ) ;
#7227 = ORIENTED_EDGE ( 'NONE', *, *, #9115, .F. ) ;
#7228 = PLANE ( 'NONE',  #10757 ) ;
#7229 = LINE ( 'NONE', #12871, #13421 ) ;
#7230 = ORIENTED_EDGE ( 'NONE', *, *, #10357, .F. ) ;
#7231 = LINE ( 'NONE', #5834, #2930 ) ;
#7232 = EDGE_CURVE ( 'NONE', #8344, #7890, #12923, .T. ) ;
#7233 = EDGE_LOOP ( 'NONE', ( #1926, #8035, #10295, #11428 ) ) ;
#7234 = CARTESIAN_POINT ( 'NONE',  ( -0.5664586606772434862, -5.586652542372875452, 2.726727161522279452 ) ) ;
#7235 = CARTESIAN_POINT ( 'NONE',  ( 2.649291707874080970, -2.243001519261071053, 4.543900225523779035 ) ) ;
#7236 = EDGE_CURVE ( 'NONE', #6119, #3213, #7113, .T. ) ;
#7237 = LINE ( 'NONE', #14188, #9991 ) ;
#7238 = DIRECTION ( 'NONE',  ( 1.224646799147350002E-16, -1.000000000000000000, -6.123233995736779594E-17 ) ) ;
#7239 = ADVANCED_FACE ( 'NONE', ( #8485 ), #10139, .F. ) ;
#7240 = DIRECTION ( 'NONE',  ( 0.7071067811865594521, 0.000000000000000000, 0.7071067811865355823 ) ) ;
#7241 = CARTESIAN_POINT ( 'NONE',  ( -0.1881942810071039751, -5.280843314568230085, 2.350674491507239949 ) ) ;
#7242 = LINE ( 'NONE', #9746, #11157 ) ;
#7243 = DIRECTION ( 'NONE',  ( -3.965082230804129973E-17, 0.000000000000000000, -1.000000000000000000 ) ) ;
#7244 = CARTESIAN_POINT ( 'NONE',  ( 1.526791597786429922, -2.774791273531720392, 6.490992212270249695 ) ) ;
#7245 = EDGE_CURVE ( 'NONE', #5452, #15809, #8583, .T. ) ;
#7246 = CARTESIAN_POINT ( 'NONE',  ( -1.102492180652080211, -3.290974492234041815, 2.968118700883599193 ) ) ;
#7247 = CARTESIAN_POINT ( 'NONE',  ( 0.7476103186298468373, -0.01779661016949178609, 2.787995836256459636 ) ) ;
#7248 = CARTESIAN_POINT ( 'NONE',  ( -0.2749999999999995781, 2.299999999999999822, 7.700000000000000178 ) ) ;
#7249 = LINE ( 'NONE', #5943, #4698 ) ;
#7250 = ORIENTED_EDGE ( 'NONE', *, *, #11877, .T. ) ;
#7251 = CARTESIAN_POINT ( 'NONE',  ( -0.2812789908084309953, -0.1557203389830509876, 7.036533610117280624 ) ) ;
#7252 = CARTESIAN_POINT ( 'NONE',  ( 0.6673090596498160165, -2.239160642901090181, 2.443133963569570355 ) ) ;
#7253 = ORIENTED_EDGE ( 'NONE', *, *, #15815, .T. ) ;
#7254 = CIRCLE ( 'NONE', #3693, 0.2500000000000002776 ) ;
#7255 = ORIENTED_EDGE ( 'NONE', *, *, #8066, .T. ) ;
#7256 = CARTESIAN_POINT ( 'NONE',  ( -2.023259452208838738, -3.174533050792599731, 3.497849062500261397 ) ) ;
#7257 = CARTESIAN_POINT ( 'NONE',  ( 0.000000000000000000, 0.000000000000000000, 0.000000000000000000 ) ) ;
#7258 = CARTESIAN_POINT ( 'NONE',  ( 2.630358833876468960, -5.368644067796615182, 4.347767980622404771 ) ) ;
#7259 = EDGE_CURVE ( 'NONE', #17154, #2052, #250, .T. ) ;
#7260 = ORIENTED_EDGE ( 'NONE', *, *, #2272, .T. ) ;
#7261 = CARTESIAN_POINT ( 'NONE',  ( 0.07299321914061039640, -0.3014830508474579673, 2.350000000000000089 ) ) ;
#7262 = VERTEX_POINT ( 'NONE', #14399 ) ;
#7263 = DIRECTION ( 'NONE',  ( 1.000000000000000000, 0.000000000000000000, 0.000000000000000000 ) ) ;
#7264 = DIRECTION ( 'NONE',  ( -1.000000000000000000, -2.018587317500279868E-16, -1.110223024625159992E-16 ) ) ;
#7265 = CARTESIAN_POINT ( 'NONE',  ( -1.520647680314179517, -1.959701183441630024, 3.320676805464663151 ) ) ;
#7266 = CARTESIAN_POINT ( 'NONE',  ( 2.500000000000000000, 2.000000000000000000, 1.600000000000000089 ) ) ;
#7267 = VERTEX_POINT ( 'NONE', #8289 ) ;
#7268 = DIRECTION ( 'NONE',  ( 0.000000000000000000, -2.220446049250320181E-15, -1.000000000000000000 ) ) ;
#7269 = CARTESIAN_POINT ( 'NONE',  ( 1.725722849164588624, -0.4023305084745772420, 5.812007984777676661 ) ) ;
#7270 = ADVANCED_FACE ( 'NONE', ( #316 ), #10467, .F. ) ;
#7271 = ORIENTED_EDGE ( 'NONE', *, *, #108, .T. ) ;
#7272 = DIRECTION ( 'NONE',  ( -1.000000000000000000, 0.000000000000000000, 0.000000000000000000 ) ) ;
#7273 = DIRECTION ( 'NONE',  ( -4.037174635000570090E-16, 0.000000000000000000, 1.000000000000000000 ) ) ;
#7274 = EDGE_CURVE ( 'NONE', #8790, #1178, #8730, .T. ) ;
#7275 = CARTESIAN_POINT ( 'NONE',  ( -1.791574935211209363, -0.1913135593220340047, 6.226029630577610163 ) ) ;
#7276 = DIRECTION ( 'NONE',  ( 2.500805593834189724E-46, 1.000000000000000000, 1.332267629550190018E-15 ) ) ;
#7277 = EDGE_CURVE ( 'NONE', #12789, #5684, #4546, .T. ) ;
#7278 = ORIENTED_EDGE ( 'NONE', *, *, #16387, .F. ) ;
#7279 = CARTESIAN_POINT ( 'NONE',  ( 1.000000000000000000, -5.599999999999999645, 5.100000000000000533 ) ) ;
#7280 = CARTESIAN_POINT ( 'NONE',  ( -1.994983296312370147, -1.334758276017820045, 5.948514050749340143 ) ) ;
#7281 = CARTESIAN_POINT ( 'NONE',  ( 1.583713126240741564, -2.429307825567371459, 6.006428174987391344 ) ) ;
#7282 = VECTOR ( 'NONE', #13044, 1000.000000000000000 ) ;
#7283 = DIRECTION ( 'NONE',  ( 2.220446049250309876E-16, 0.000000000000000000, -1.000000000000000000 ) ) ;
#7284 = EDGE_CURVE ( 'NONE', #4993, #3917, #811, .T. ) ;
#7285 = ORIENTED_EDGE ( 'NONE', *, *, #2012, .F. ) ;
#7286 = LINE ( 'NONE', #157, #839 ) ;
#7287 = CARTESIAN_POINT ( 'NONE',  ( 1.925836318347889931, -0.4112288135593234473, 6.525927015348126581 ) ) ;
#7288 = CARTESIAN_POINT ( 'NONE',  ( 2.192143888961729736, -4.218665147405599392, 5.556300681753580051 ) ) ;
#7289 = FACE_OUTER_BOUND ( 'NONE', #16908, .T. ) ;
#7290 = CARTESIAN_POINT ( 'NONE',  ( 1.899999999999999911, 2.000000000000000000, 1.600000000000000089 ) ) ;
#7291 = CARTESIAN_POINT ( 'NONE',  ( 1.666450993087180477, -5.117584745762705722, 6.765380371283858274 ) ) ;
#7292 = VERTEX_POINT ( 'NONE', #9075 ) ;
#7293 = ORIENTED_EDGE ( 'NONE', *, *, #11294, .F. ) ;
#7294 = DIRECTION ( 'NONE',  ( 0.7071067811865470176, 0.000000000000000000, 0.7071067811865480168 ) ) ;
#7295 = PLANE ( 'NONE',  #18248 ) ;
#7296 = VECTOR ( 'NONE', #12244, 1000.000000000000000 ) ;
#7297 = VERTEX_POINT ( 'NONE', #1701 ) ;
#7298 = AXIS2_PLACEMENT_3D ( 'NONE', #17794, #779, #10589 ) ;
#7299 = CARTESIAN_POINT ( 'NONE',  ( 1.652654650382400003, -0.7952867690272209522, 3.029252778805620050 ) ) ;
#7300 = CARTESIAN_POINT ( 'NONE',  ( -0.1749999999999999889, 9.299999999999998934, 0.5999999999999999778 ) ) ;
#7301 = CARTESIAN_POINT ( 'NONE',  ( 2.159566522375460096, -2.359442960702510028, 5.635424033751039730 ) ) ;
#7302 = AXIS2_PLACEMENT_3D ( 'NONE', #14035, #9876, #10058 ) ;
#7303 = EDGE_CURVE ( 'NONE', #5456, #8719, #483, .T. ) ;
#7304 = CARTESIAN_POINT ( 'NONE',  ( 0.2134934900267039248, -5.004947479095229745, 2.650814970067049803 ) ) ;
#7305 = CARTESIAN_POINT ( 'NONE',  ( -1.558664967382870525, -1.540511994252448780, 6.847947208954447973 ) ) ;
#7306 = CARTESIAN_POINT ( 'NONE',  ( 1.438959988998139914E-16, -0.1499999999999999944, 2.350000000000000089 ) ) ;
#7307 = CARTESIAN_POINT ( 'NONE',  ( -2.004091155098381094, -4.963890372630814340, 4.254443623407394348 ) ) ;
#7308 = CIRCLE ( 'NONE', #5228, 0.8000000000000000444 ) ;
#7309 = CARTESIAN_POINT ( 'NONE',  ( -1.791574935211209807, -0.4913135593220339659, 6.226029630577610163 ) ) ;
#7310 = LINE ( 'NONE', #17193, #12331 ) ;
#7311 = AXIS2_PLACEMENT_3D ( 'NONE', #5671, #4175, #12881 ) ;
#7312 = CARTESIAN_POINT ( 'NONE',  ( 2.203023580853990193, -0.3578389830508479919, 3.872235369154280349 ) ) ;
#7313 = LINE ( 'NONE', #2017, #13900 ) ;
#7314 = ORIENTED_EDGE ( 'NONE', *, *, #7643, .T. ) ;
#7315 = PLANE ( 'NONE',  #2192 ) ;
#7316 = EDGE_LOOP ( 'NONE', ( #476, #8406, #869, #6963 ) ) ;
#7317 = EDGE_CURVE ( 'NONE', #6834, #14013, #11464, .T. ) ;
#7318 = CARTESIAN_POINT ( 'NONE',  ( -0.3367924244280810497, 2.254758922476410188, 7.700000000000000178 ) ) ;
#7319 = LINE ( 'NONE', #11567, #8828 ) ;
#7320 = VECTOR ( 'NONE', #14451, 1000.000000000000000 ) ;
#7321 = VERTEX_POINT ( 'NONE', #17415 ) ;
#7322 = CARTESIAN_POINT ( 'NONE',  ( -2.046424002475610404, -5.528813559322025561, 4.536201610417774255 ) ) ;
#7323 = LINE ( 'NONE', #14449, #9435 ) ;
#7324 = CARTESIAN_POINT ( 'NONE',  ( -2.282375681463830297, -3.174533050792599731, 3.345793611865449435 ) ) ;
#7325 = AXIS2_PLACEMENT_3D ( 'NONE', #14500, #10408, #14316 ) ;
#7326 = CARTESIAN_POINT ( 'NONE',  ( -0.009452110982656868748, -5.299807955295460005, 2.350000000000000089 ) ) ;
#7327 = VECTOR ( 'NONE', #8686, 1000.000000000000000 ) ;
#7328 = DIRECTION ( 'NONE',  ( -1.224646799147350002E-16, 8.383884571949770538E-16, -1.000000000000000000 ) ) ;
#7329 = DIRECTION ( 'NONE',  ( -6.049014748177250683E-16, 2.493473113004675144E-16, -1.000000000000000000 ) ) ;
#7330 = DIRECTION ( 'NONE',  ( 0.000000000000000000, 0.000000000000000000, 1.000000000000000000 ) ) ;
#7331 = CARTESIAN_POINT ( 'NONE',  ( -2.334032080503389839, -3.310421904162350160, 5.001728246382240783 ) ) ;
#7332 = VECTOR ( 'NONE', #17734, 1000.000000000000000 ) ;
#7333 = CARTESIAN_POINT ( 'NONE',  ( 1.440522616026430391, -0.7952867690272208412, 3.241384813161591438 ) ) ;
#7334 = VECTOR ( 'NONE', #3531, 1000.000000000000000 ) ;
#7335 = CARTESIAN_POINT ( 'NONE',  ( -2.058670345754650022, -0.2491525423728820077, 3.559656372813929881 ) ) ;
#7336 = EDGE_CURVE ( 'NONE', #3539, #4745, #12995, .T. ) ;
#7337 = DIRECTION ( 'NONE',  ( 2.220446049250309876E-16, 0.000000000000000000, -1.000000000000000000 ) ) ;
#7338 = EDGE_CURVE ( 'NONE', #1995, #8433, #11597, .T. ) ;
#7339 = DIRECTION ( 'NONE',  ( 0.000000000000000000, 0.000000000000000000, -1.000000000000000000 ) ) ;
#7340 = ORIENTED_EDGE ( 'NONE', *, *, #4091, .T. ) ;
#7341 = CARTESIAN_POINT ( 'NONE',  ( 1.788074174585509768, -3.617010528270069525, 2.738902236199779239 ) ) ;
#7342 = ADVANCED_FACE ( 'NONE', ( #3345 ), #4735, .T. ) ;
#7343 = AXIS2_PLACEMENT_3D ( 'NONE', #9202, #7926, #13577 ) ;
#7344 = CARTESIAN_POINT ( 'NONE',  ( -1.289141334274979789, -0.1824152542372889096, 6.297747079672432413 ) ) ;
#7345 = CARTESIAN_POINT ( 'NONE',  ( 2.211317922628870392, -2.472043525783979678, 3.894507149290419967 ) ) ;
#7346 = ORIENTED_EDGE ( 'NONE', *, *, #16845, .F. ) ;
#7347 = ADVANCED_FACE ( 'NONE', ( #5955 ), #8990, .F. ) ;
#7348 = ORIENTED_EDGE ( 'NONE', *, *, #653, .F. ) ;
#7349 = CARTESIAN_POINT ( 'NONE',  ( -0.01716182025094739605, -3.430704221963769562, 2.346608583467349796 ) ) ;
#7350 = APPLICATION_PROTOCOL_DEFINITION ( 'draft international standard', 'automotive_design', 1998, #4946 ) ;
#7351 = CARTESIAN_POINT ( 'NONE',  ( -1.128670402850159737, -5.170974576271189171, 7.101865548313641696 ) ) ;
#7352 = CIRCLE ( 'NONE', #2016, 0.6100000000000000977 ) ;
#7353 = CIRCLE ( 'NONE', #6703, 0.7211102550927981358 ) ;
#7354 = ORIENTED_EDGE ( 'NONE', *, *, #3866, .F. ) ;
#7355 = DIRECTION ( 'NONE',  ( -1.000000000000000000, 0.000000000000000000, 0.000000000000000000 ) ) ;
#7356 = CARTESIAN_POINT ( 'NONE',  ( -0.9707742057416274273, -0.4735169491525429986, 6.508944043303927174 ) ) ;
#7357 = ORIENTED_EDGE ( 'NONE', *, *, #6133, .T. ) ;
#7358 = VECTOR ( 'NONE', #3616, 1000.000000000000000 ) ;
#7359 = LINE ( 'NONE', #15782, #9694 ) ;
#7360 = CARTESIAN_POINT ( 'NONE',  ( 1.959085573314239159, -2.635061543801990869, 5.313910057793555630 ) ) ;
#7361 = LINE ( 'NONE', #408, #11167 ) ;
#7362 = CARTESIAN_POINT ( 'NONE',  ( 2.268288188848061715, -0.3489406779661023417, 3.322421079292310786 ) ) ;
#7363 = ORIENTED_EDGE ( 'NONE', *, *, #9175, .T. ) ;
#7364 = CARTESIAN_POINT ( 'NONE',  ( 2.500000000000000000, 2.000000000000000000, 1.600000000000000089 ) ) ;
#7365 = AXIS2_PLACEMENT_3D ( 'NONE', #11540, #5802, #14586 ) ;
#7366 = LINE ( 'NONE', #11429, #17096 ) ;
#7367 = VECTOR ( 'NONE', #7163, 1000.000000000000000 ) ;
#7368 = EDGE_CURVE ( 'NONE', #8925, #17576, #10385, .T. ) ;
#7369 = CARTESIAN_POINT ( 'NONE',  ( 1.661700935788380074, -5.337500000000000355, 3.038299064211610112 ) ) ;
#7370 = ORIENTED_EDGE ( 'NONE', *, *, #11743, .F. ) ;
#7371 = CARTESIAN_POINT ( 'NONE',  ( -0.6964468257805866980, -5.466525423728811006, 6.631228347243847132 ) ) ;
#7372 = SURFACE_SIDE_STYLE ('',( #17240 ) ) ;
#7373 = CARTESIAN_POINT ( 'NONE',  ( -1.713314936023349722, -0.2610169491525430319, 3.089913064446579760 ) ) ;
#7374 = CARTESIAN_POINT ( 'NONE',  ( -1.449568901432419343, -0.5625000000000005551, 3.250431098567584165 ) ) ;
#7375 = CARTESIAN_POINT ( 'NONE',  ( 2.607432201095279733, -4.078935417675873865, 4.205620581240154365 ) ) ;
#7376 = ORIENTED_EDGE ( 'NONE', *, *, #10570, .T. ) ;
#7377 = DIRECTION ( 'NONE',  ( 0.000000000000000000, -1.000000000000000000, 0.000000000000000000 ) ) ;
#7378 = VECTOR ( 'NONE', #7955, 1000.000000000000114 ) ;
#7379 = CARTESIAN_POINT ( 'NONE',  ( 1.781655196750449921, -2.079983501243049648, 3.162323035427780482 ) ) ;
#7380 = DIRECTION ( 'NONE',  ( 0.000000000000000000, -1.000000000000000000, 2.493473113004670213E-16 ) ) ;
#7381 = CARTESIAN_POINT ( 'NONE',  ( -1.712910428781911021, -2.895073591333140239, 5.831741890007735130 ) ) ;
#7382 = DIRECTION ( 'NONE',  ( -1.000000000000000000, 0.000000000000000000, 6.123233995736769734E-17 ) ) ;
#7383 = PRODUCT_DEFINITION_FORMATION_WITH_SPECIFIED_SOURCE ( 'ANY', '', #7704, .NOT_KNOWN. ) ;
#7384 = ORIENTED_EDGE ( 'NONE', *, *, #10722, .F. ) ;
#7385 = ADVANCED_FACE ( 'NONE', ( #3174 ), #8830, .F. ) ;
#7386 = CARTESIAN_POINT ( 'NONE',  ( 2.500000000000000000, 7.299999999999999822, 0.6099999999999999867 ) ) ;
#7387 = AXIS2_PLACEMENT_3D ( 'NONE', #15953, #2037, #17564 ) ;
#7388 = CARTESIAN_POINT ( 'NONE',  ( -2.349129089426440054, -4.894025507765950245, 4.842612091679129982 ) ) ;
#7389 = CARTESIAN_POINT ( 'NONE',  ( 1.550000000000000044, -6.000000000000000000, 6.100000000000000533 ) ) ;
#7390 = CARTESIAN_POINT ( 'NONE',  ( -0.5500000000000000444, 3.050000000000000266, 2.699264068711930253 ) ) ;
#7391 = CARTESIAN_POINT ( 'NONE',  ( 0.3171869470818560743, -5.144279661016955885, 7.334814496515233095 ) ) ;
#7392 = ORIENTED_EDGE ( 'NONE', *, *, #5168, .F. ) ;
#7393 = EDGE_LOOP ( 'NONE', ( #17224, #12768, #2511, #1301 ) ) ;
#7394 = LINE ( 'NONE', #438, #13320 ) ;
#7395 = PLANE ( 'NONE',  #6720 ) ;
#7396 = ORIENTED_EDGE ( 'NONE', *, *, #5013, .T. ) ;
#7397 = FACE_OUTER_BOUND ( 'NONE', #14676, .T. ) ;
#7398 = CARTESIAN_POINT ( 'NONE',  ( 2.035218756299218779, -0.8185750573155082810, 2.996768277952650106 ) ) ;
#7399 = CARTESIAN_POINT ( 'NONE',  ( 1.670747221194369914, -0.4963798976394459550, 3.047345349617600174 ) ) ;
#7400 = CARTESIAN_POINT ( 'NONE',  ( -0.3042893218813459977, 6.450000000000000178, 2.029289321881350361 ) ) ;
#7401 = VECTOR ( 'NONE', #9799, 1000.000000000000000 ) ;
#7402 = CARTESIAN_POINT ( 'NONE',  ( 0.3159454637157339540, -2.615614131873679860, 7.032150113402090064 ) ) ;
#7403 = FACE_OUTER_BOUND ( 'NONE', #5681, .T. ) ;
#7404 = CARTESIAN_POINT ( 'NONE',  ( 2.584100759211419795, -0.9350164987569505870, 4.095403473953104445 ) ) ;
#7405 = FACE_BOUND ( 'NONE', #5772, .T. ) ;
#7406 = DIRECTION ( 'NONE',  ( 1.000000000000000000, 0.000000000000000000, -7.401486830834380223E-16 ) ) ;
#7407 = CARTESIAN_POINT ( 'NONE',  ( 0.6628679656440349399, 6.450000000000000178, 1.670710678118660031 ) ) ;
#7408 = EDGE_LOOP ( 'NONE', ( #7354, #4163, #6063, #6777 ) ) ;
#7409 = ORIENTED_EDGE ( 'NONE', *, *, #12418, .F. ) ;
#7410 = CARTESIAN_POINT ( 'NONE',  ( 1.889999999999999902, 7.299999999999999822, 0.5999999999999999778 ) ) ;
#7411 = AXIS2_PLACEMENT_3D ( 'NONE', #11826, #3035, #4767 ) ;
#7412 = PLANE ( 'NONE',  #15051 ) ;
#7413 = EDGE_CURVE ( 'NONE', #13613, #16121, #13084, .T. ) ;
#7414 = ORIENTED_EDGE ( 'NONE', *, *, #15014, .T. ) ;
#7415 = CARTESIAN_POINT ( 'NONE',  ( -0.3803919826357066158, -5.291101694915254505, 2.682580100125310896 ) ) ;
#7416 = DIRECTION ( 'NONE',  ( 2.590520390792030218E-15, 0.000000000000000000, -1.000000000000000000 ) ) ;
#7417 = CARTESIAN_POINT ( 'NONE',  ( -2.340959815966380031, -1.750106588847040179, 4.942183458383479611 ) ) ;
#7418 = CARTESIAN_POINT ( 'NONE',  ( 0.2266049403549809660, -3.453992510252061887, 2.055805624767989226 ) ) ;
#7419 = DIRECTION ( 'NONE',  ( -6.049014748177260544E-16, 0.000000000000000000, -1.000000000000000000 ) ) ;
#7420 = CARTESIAN_POINT ( 'NONE',  ( 1.661700935788380074, -5.337500000000000355, 3.038299064211610112 ) ) ;
#7421 = DIRECTION ( 'NONE',  ( 4.440892098500630106E-16, 0.000000000000000000, -1.000000000000000000 ) ) ;
#7422 = CARTESIAN_POINT ( 'NONE',  ( 2.226511124464869873, -1.074746228486680000, 5.462491901673799610 ) ) ;
#7423 = LINE ( 'NONE', #115, #8841 ) ;
#7424 = AXIS2_PLACEMENT_3D ( 'NONE', #11373, #8678, #18189 ) ;
#7425 = CARTESIAN_POINT ( 'NONE',  ( 2.337178851518220135, -2.588484967225419986, 4.976298214796759822 ) ) ;
#7426 = CARTESIAN_POINT ( 'NONE',  ( -1.566607907718199577, -4.432100618360157007, 6.026891670824300107 ) ) ;
#7427 = FACE_OUTER_BOUND ( 'NONE', #16262, .T. ) ;
#7428 = CARTESIAN_POINT ( 'NONE',  ( -2.616666666666669805, -4.318079751576579732E-16, 4.000000000000000000 ) ) ;
#7429 = ORIENTED_EDGE ( 'NONE', *, *, #12538, .T. ) ;
#7430 = CARTESIAN_POINT ( 'NONE',  ( 2.639965200365849363, -3.849893411152959910, 4.971472712918224346 ) ) ;
#7431 = CARTESIAN_POINT ( 'NONE',  ( 1.202278654260740876, -0.1201271186440679706, 6.364093491318035589 ) ) ;
#7432 = CARTESIAN_POINT ( 'NONE',  ( 2.276802572547980130, -2.495331814072260013, 4.104251954998760610 ) ) ;
#7433 = ORIENTED_EDGE ( 'NONE', *, *, #16055, .F. ) ;
#7434 = VERTEX_POINT ( 'NONE', #3425 ) ;
#7435 = DIRECTION ( 'NONE',  ( 1.000000000000000000, 0.000000000000000000, -7.273661547324610053E-16 ) ) ;
#7436 = VERTEX_POINT ( 'NONE', #17574 ) ;
#7437 = CARTESIAN_POINT ( 'NONE',  ( 0.2023972492402060508, -3.453992510252061443, 2.355265251465770149 ) ) ;
#7438 = APPLICATION_PROTOCOL_DEFINITION ( 'draft international standard', 'automotive_design', 1998, #15980 ) ;
#7439 = CARTESIAN_POINT ( 'NONE',  ( -1.192209327851089240, -5.577754237288145234, 2.329031440774910422 ) ) ;
#7440 = ORIENTED_EDGE ( 'NONE', *, *, #1271, .T. ) ;
#7441 = DIRECTION ( 'NONE',  ( -1.850371707708599740E-16, -1.000000000000000000, -9.251858538542959255E-17 ) ) ;
#7442 = CARTESIAN_POINT ( 'NONE',  ( -1.300961508564169922, -0.4779661016949160457, 6.661123742937279602 ) ) ;
#7443 = ORIENTED_EDGE ( 'NONE', *, *, #1822, .T. ) ;
#7444 = EDGE_CURVE ( 'NONE', #15692, #11846, #16485, .T. ) ;
#7445 = CARTESIAN_POINT ( 'NONE',  ( 1.399999999999999911, -5.500000000000000000, 6.100000000000000533 ) ) ;
#7446 = DIRECTION ( 'NONE',  ( -2.220446049250319983E-16, 0.000000000000000000, -1.000000000000000000 ) ) ;
#7447 = EDGE_CURVE ( 'NONE', #14738, #1479, #17499, .T. ) ;
#7448 = CARTESIAN_POINT ( 'NONE',  ( 0.5805547688318586363, -2.239160642901089293, 2.730772231808960449 ) ) ;
#7449 = EDGE_CURVE ( 'NONE', #3897, #4403, #4817, .T. ) ;
#7450 = CARTESIAN_POINT ( 'NONE',  ( 2.268288188848061715, -0.04894067796610205440, 3.322421079292310786 ) ) ;
#7451 = ORIENTED_EDGE ( 'NONE', *, *, #16364, .F. ) ;
#7452 = DIRECTION ( 'NONE',  ( -1.000000000000000000, 0.000000000000000000, -1.739311637268509859E-16 ) ) ;
#7453 = CARTESIAN_POINT ( 'NONE',  ( 1.438959988998139914E-16, -0.1499999999999999944, 2.350000000000000089 ) ) ;
#7454 = CARTESIAN_POINT ( 'NONE',  ( 0.6964468257805941365, -0.4334745762711874617, 6.631228347243847132 ) ) ;
#7455 = VERTEX_POINT ( 'NONE', #16047 ) ;
#7456 = LINE ( 'NONE', #13097, #13023 ) ;
#7457 = CARTESIAN_POINT ( 'NONE',  ( 0.6187874668174475623, -5.435381355932195291, 6.657494107589526422 ) ) ;
#7458 = LINE ( 'NONE', #4662, #14715 ) ;
#7459 = LINE ( 'NONE', #1888, #13926 ) ;
#7460 = CARTESIAN_POINT ( 'NONE',  ( -2.435897774776361491, -3.240557039297494057, 5.753335522918235689 ) ) ;
#7461 = ORIENTED_EDGE ( 'NONE', *, *, #13034, .T. ) ;
#7462 = CARTESIAN_POINT ( 'NONE',  ( 2.111627294540149968, -3.710163681423230386, 3.660877362176659933 ) ) ;
#7463 = EDGE_CURVE ( 'NONE', #7208, #4205, #16127, .T. ) ;
#7464 = CARTESIAN_POINT ( 'NONE',  ( 1.800000000000000044, 11.29999999999999893, 1.600000000000000089 ) ) ;
#7465 = CARTESIAN_POINT ( 'NONE',  ( -1.366362128262280429, -1.684082600342149627, 3.167695729602423516 ) ) ;
#7466 = CARTESIAN_POINT ( 'NONE',  ( 2.500000000000000000, 11.29999999999999893, 7.649999999999999467 ) ) ;
#7467 = EDGE_LOOP ( 'NONE', ( #12808, #7943, #3858, #17637 ) ) ;
#7468 = LINE ( 'NONE', #6064, #3448 ) ;
#7469 = DIRECTION ( 'NONE',  ( -0.7071067811865480168, 0.000000000000000000, 0.7071067811865470176 ) ) ;
#7470 = CARTESIAN_POINT ( 'NONE',  ( -1.579331079541819394, -1.241605122864670285, 6.832797935622397567 ) ) ;
#7471 = CARTESIAN_POINT ( 'NONE',  ( 0.1824815401350060040, -4.498124606865050445, 7.046368721022729709 ) ) ;
#7472 = FACE_OUTER_BOUND ( 'NONE', #3288, .T. ) ;
#7473 = DIRECTION ( 'NONE',  ( -1.224646799147351975E-16, 1.000000000000000000, 6.123233995736759873E-17 ) ) ;
#7474 = CARTESIAN_POINT ( 'NONE',  ( 2.058670345754650022, -5.050847457627120285, 3.559656372813920111 ) ) ;
#7475 = ORIENTED_EDGE ( 'NONE', *, *, #3951, .F. ) ;
#7476 = ORIENTED_EDGE ( 'NONE', *, *, #6014, .T. ) ;
#7477 = CARTESIAN_POINT ( 'NONE',  ( 0.5372984490435490645, 4.599999999999999645, 7.700000000000000178 ) ) ;
#7478 = CARTESIAN_POINT ( 'NONE',  ( 1.438959988998139914E-16, -0.2999999999999999889, 2.350000000000000089 ) ) ;
#7479 = ORIENTED_EDGE ( 'NONE', *, *, #2935, .T. ) ;
#7480 = CARTESIAN_POINT ( 'NONE',  ( 2.531332855772549184, -2.635061543801990869, 5.497162258444460825 ) ) ;
#7481 = EDGE_CURVE ( 'NONE', #5167, #1590, #12429, .T. ) ;
#7482 = DIRECTION ( 'NONE',  ( -1.000000000000000000, 1.480297366166879989E-15, 0.000000000000000000 ) ) ;
#7483 = AXIS2_PLACEMENT_3D ( 'NONE', #11368, #15547, #1559 ) ;
#7484 = LINE ( 'NONE', #17187, #8503 ) ;
#7485 = CARTESIAN_POINT ( 'NONE',  ( -0.6096110657044609971, -1.800524041783589935, 2.426869991387519576 ) ) ;
#7486 = CARTESIAN_POINT ( 'NONE',  ( 0.6410058658986126368, -5.311531839079355777, 2.106117395030960626 ) ) ;
#7487 = CARTESIAN_POINT ( 'NONE',  ( 2.579602008086750775, -1.051457940198389673, 5.323511966907245707 ) ) ;
#7488 = CARTESIAN_POINT ( 'NONE',  ( 0.5500000000000000444, 2.050000000000000266, 1.600000000000000089 ) ) ;
#7489 = CARTESIAN_POINT ( 'NONE',  ( -2.051973656473811136, -4.917313796054240349, 4.634380218157504672 ) ) ;
#7490 = CARTESIAN_POINT ( 'NONE',  ( 2.318251751302029984, -0.3667372881355940306, 4.294764266798990704 ) ) ;
#7491 = DIRECTION ( 'NONE',  ( -1.000000000000000000, 0.000000000000000000, 6.123233995736769734E-17 ) ) ;
#7492 = ORIENTED_EDGE ( 'NONE', *, *, #12897, .F. ) ;
#7493 = VECTOR ( 'NONE', #1739, 1000.000000000000000 ) ;
#7494 = CARTESIAN_POINT ( 'NONE',  ( 0.1749999999999999889, 4.299999999999999822, 1.600000000000000089 ) ) ;
#7495 = EDGE_LOOP ( 'NONE', ( #3037, #16211, #14151, #13802 ) ) ;
#7496 = CARTESIAN_POINT ( 'NONE',  ( 1.289999999999999813, 7.900000000000003908, 2.878305776370009209E-15 ) ) ;
#7497 = PLANE ( 'NONE',  #841 ) ;
#7498 = ORIENTED_EDGE ( 'NONE', *, *, #14566, .F. ) ;
#7499 = DIRECTION ( 'NONE',  ( -1.000000000000000000, 0.000000000000000000, 0.000000000000000000 ) ) ;
#7500 = CARTESIAN_POINT ( 'NONE',  ( -1.145304265383870090, -3.077539021279469988, 6.755972720436099088 ) ) ;
#7501 = EDGE_CURVE ( 'NONE', #14262, #12160, #5304, .T. ) ;
#7502 = DIRECTION ( 'NONE',  ( 0.000000000000000000, -1.000000000000000000, 0.000000000000000000 ) ) ;
#7503 = CARTESIAN_POINT ( 'NONE',  ( -2.500000000000000000, 11.15000000000000036, 1.600000000000000089 ) ) ;
#7504 = CARTESIAN_POINT ( 'NONE',  ( 0.7109160811436110450, -1.307629111369560171, 6.943511536198400336 ) ) ;
#7505 = CARTESIAN_POINT ( 'NONE',  ( 2.311987889326980294, -4.078935417675859654, 4.260161748947079552 ) ) ;
#7506 = CARTESIAN_POINT ( 'NONE',  ( 1.572563554680340703, -0.8185750573155082810, 3.380172092915559645 ) ) ;
#7507 = CARTESIAN_POINT ( 'NONE',  ( 0.7983658734558030101, -0.4334745762711870176, 6.913847129767330735 ) ) ;
#7508 = DIRECTION ( 'NONE',  ( -1.000000000000000000, -1.189524669241239855E-16, -4.716563129111599823E-33 ) ) ;
#7509 = DIRECTION ( 'NONE',  ( 6.123233995736769734E-17, 0.000000000000000000, 1.000000000000000000 ) ) ;
#7510 = VERTEX_POINT ( 'NONE', #16598 ) ;
#7511 = CARTESIAN_POINT ( 'NONE',  ( -1.679950111053631900, -0.1957627118644069686, 5.880020650119711867 ) ) ;
#7512 = CARTESIAN_POINT ( 'NONE',  ( 1.219286470748990103, -4.381683165423610582, 6.712979431025659416 ) ) ;
#7513 = AXIS2_PLACEMENT_3D ( 'NONE', #1666, #8432, #14442 ) ;
#7514 = ORIENTED_EDGE ( 'NONE', *, *, #10489, .T. ) ;
#7515 = ORIENTED_EDGE ( 'NONE', *, *, #6236, .F. ) ;
#7516 = DIRECTION ( 'NONE',  ( 0.000000000000000000, 0.000000000000000000, 1.000000000000000000 ) ) ;
#7517 = ORIENTED_EDGE ( 'NONE', *, *, #10613, .F. ) ;
#7518 = CARTESIAN_POINT ( 'NONE',  ( -2.226511124464849445, -4.525253771513309431, 5.462491901673850236 ) ) ;
#7519 = APPLICATION_PROTOCOL_DEFINITION ( 'draft international standard', 'automotive_design', 1998, #6861 ) ;
#7520 = CARTESIAN_POINT ( 'NONE',  ( 2.321479326063749404, -5.050847457627124726, 3.414080590619961608 ) ) ;
#7521 = DIRECTION ( 'NONE',  ( 1.000000000000000000, -1.224646799147350002E-16, 0.000000000000000000 ) ) ;
#7522 = CARTESIAN_POINT ( 'NONE',  ( -0.9150601050661559821, -0.4690677966101700069, 6.868218666554230190 ) ) ;
#7523 = VERTEX_POINT ( 'NONE', #14837 ) ;
#7524 = PLANE ( 'NONE',  #2290 ) ;
#7525 = DIRECTION ( 'NONE',  ( -4.440892098500630106E-16, 0.000000000000000000, -1.000000000000000000 ) ) ;
#7526 = VECTOR ( 'NONE', #17469, 1000.000000000000000 ) ;
#7527 = CARTESIAN_POINT ( 'NONE',  ( -2.028464043723881005, -4.870737219477664581, 5.016599851465114668 ) ) ;
#7528 = CARTESIAN_POINT ( 'NONE',  ( 2.540842781840729536, -0.08898305084745804228, 5.466141598148674952 ) ) ;
#7529 = ORIENTED_EDGE ( 'NONE', *, *, #8010, .F. ) ;
#7530 = LINE ( 'NONE', #14303, #10541 ) ;
#7531 = ORIENTED_EDGE ( 'NONE', *, *, #8286, .T. ) ;
#7532 = FACE_OUTER_BOUND ( 'NONE', #2229, .T. ) ;
#7533 = CARTESIAN_POINT ( 'NONE',  ( -2.116444151961480280, -5.546610169491529518, 3.670839500609359707 ) ) ;
#7534 = EDGE_CURVE ( 'NONE', #16854, #15324, #2299, .T. ) ;
#7535 = CARTESIAN_POINT ( 'NONE',  ( 13.63407075111029876, 11.40000000000000036, 9.955530934770520091 ) ) ;
#7536 = EDGE_CURVE ( 'NONE', #14839, #17750, #4353, .T. ) ;
#7537 = CARTESIAN_POINT ( 'NONE',  ( -1.217041937262000051, -0.2742238837839079402, 2.666998181419179659 ) ) ;
#7538 = CARTESIAN_POINT ( 'NONE',  ( 1.579331079541870686, -4.358394877135324030, 6.832797935622368257 ) ) ;
#7539 = ORIENTED_EDGE ( 'NONE', *, *, #3828, .T. ) ;
#7540 = CARTESIAN_POINT ( 'NONE',  ( -2.245209214543380405, -2.964938456197999894, 5.405536158119060630 ) ) ;
#7541 = CARTESIAN_POINT ( 'NONE',  ( 1.652654650382400003, -0.7952867690272209522, 3.029252778805629820 ) ) ;
#7542 = LINE ( 'NONE', #13371, #11613 ) ;
#7543 = FACE_OUTER_BOUND ( 'NONE', #4975, .T. ) ;
#7544 = DIRECTION ( 'NONE',  ( -1.000000000000000000, 0.000000000000000000, 4.318427418585891014E-15 ) ) ;
#7545 = CARTESIAN_POINT ( 'NONE',  ( 0.03895741673415010348, -1.870388906648449812, 2.647347042895590086 ) ) ;
#7546 = ORIENTED_EDGE ( 'NONE', *, *, #2275, .F. ) ;
#7547 = ADVANCED_FACE ( 'NONE', ( #4082 ), #15677, .T. ) ;
#7548 = CARTESIAN_POINT ( 'NONE',  ( -1.889999999999999902, 8.500000000000000000, 0.5999999999999999778 ) ) ;
#7549 = CARTESIAN_POINT ( 'NONE',  ( 2.006003143956041068, -0.8689925102520592581, 6.437545705712618194 ) ) ;
#7550 = VERTEX_POINT ( 'NONE', #11032 ) ;
#7551 = CARTESIAN_POINT ( 'NONE',  ( 1.728413393879709936, -4.311818300558750039, 6.297289212178290185 ) ) ;
#7552 = LINE ( 'NONE', #3376, #14305 ) ;
#7553 = EDGE_CURVE ( 'NONE', #8624, #2681, #8509, .T. ) ;
#7554 = CARTESIAN_POINT ( 'NONE',  ( 1.000000000000000000, -6.000000000000000000, 5.100000000000000533 ) ) ;
#7555 = CARTESIAN_POINT ( 'NONE',  ( -2.354888465609351389, -5.202118644067803999, 5.923664702843871588 ) ) ;
#7556 = VERTEX_POINT ( 'NONE', #9833 ) ;
#7557 = EDGE_CURVE ( 'NONE', #8790, #12277, #4644, .T. ) ;
#7558 = ORIENTED_EDGE ( 'NONE', *, *, #13367, .F. ) ;
#7559 = CARTESIAN_POINT ( 'NONE',  ( 0.5921572875253799939, 6.450000000000000178, 1.600000000000000089 ) ) ;
#7560 = EDGE_CURVE ( 'NONE', #16101, #1588, #4174, .T. ) ;
#7561 = DIRECTION ( 'NONE',  ( 1.644774851296529842E-16, -1.000000000000000000, 0.000000000000000000 ) ) ;
#7562 = ADVANCED_FACE ( 'NONE', ( #13910 ), #1504, .T. ) ;
#7563 = ORIENTED_EDGE ( 'NONE', *, *, #17653, .T. ) ;
#7564 = CARTESIAN_POINT ( 'NONE',  ( 0.2683982510036849733, -2.192584066324520187, 2.059720455735791322 ) ) ;
#7565 = VECTOR ( 'NONE', #1207, 1000.000000000000000 ) ;
#7566 = FACE_OUTER_BOUND ( 'NONE', #13919, .T. ) ;
#7567 = CARTESIAN_POINT ( 'NONE',  ( 2.500000000000000000, 4.700000000000000178, 0.6099999999999999867 ) ) ;
#7568 = CARTESIAN_POINT ( 'NONE',  ( -2.245209214543380405, -2.964938456197999894, 5.405536158119060630 ) ) ;
#7569 = CARTESIAN_POINT ( 'NONE',  ( 0.5070585469427659753, -5.011796459788054214, 2.696565570857651473 ) ) ;
#7570 = CARTESIAN_POINT ( 'NONE',  ( -2.358786130709981332, -1.656953435693890864, 5.916240799583737164 ) ) ;
#7571 = DIRECTION ( 'NONE',  ( 1.000000000000000000, -1.762990951820104838E-17, 2.220446049250309876E-16 ) ) ;
#7572 = DIRECTION ( 'NONE',  ( 0.000000000000000000, -1.000000000000000000, -1.359631073446889961E-32 ) ) ;
#7573 = CARTESIAN_POINT ( 'NONE',  ( 1.851073041990159984, -0.4067796610169499560, 6.153284478378259870 ) ) ;
#7574 = CARTESIAN_POINT ( 'NONE',  ( 1.836970198721020197E-17, 3.581751045813930112, 7.700000000000000178 ) ) ;
#7575 = ORIENTED_EDGE ( 'NONE', *, *, #8015, .T. ) ;
#7576 = EDGE_CURVE ( 'NONE', #7455, #5117, #12880, .T. ) ;
#7577 = VECTOR ( 'NONE', #17418, 1000.000000000000000 ) ;
#7578 = DIRECTION ( 'NONE',  ( -5.865000419954259844E-16, 9.550139141648499357E-32, -1.000000000000000000 ) ) ;
#7579 = ORIENTED_EDGE ( 'NONE', *, *, #8688, .F. ) ;
#7580 = DIRECTION ( 'NONE',  ( -1.000000000000000000, 0.000000000000000000, 0.000000000000000000 ) ) ;
#7581 = CARTESIAN_POINT ( 'NONE',  ( 13.63407075111029876, 12.00000000000000000, 9.955530934770520091 ) ) ;
#7582 = ORIENTED_EDGE ( 'NONE', *, *, #14353, .F. ) ;
#7583 = DIRECTION ( 'NONE',  ( 1.000000000000000000, 0.000000000000000000, 0.000000000000000000 ) ) ;
#7584 = CARTESIAN_POINT ( 'NONE',  ( 0.01716182025089369942, -2.169295778036230082, 2.346608583467340026 ) ) ;
#7585 = SURFACE_SIDE_STYLE ('',( #8974 ) ) ;
#7586 = DIRECTION ( 'NONE',  ( 6.771944841082658606E-17, -4.886939904639989483E-32, 1.000000000000000000 ) ) ;
#7587 = VECTOR ( 'NONE', #6917, 1000.000000000000000 ) ;
#7588 = EDGE_CURVE ( 'NONE', #14363, #18075, #513, .T. ) ;
#7589 = CARTESIAN_POINT ( 'NONE',  ( -2.255259958075430227, -1.703530012270459970, 5.372717034856060003 ) ) ;
#7590 = AXIS2_PLACEMENT_3D ( 'NONE', #1625, #12911, #5880 ) ;
#7591 = CARTESIAN_POINT ( 'NONE',  ( 1.991984774470479946, -3.985782264522710339, 3.446707398186009907 ) ) ;
#7592 = CARTESIAN_POINT ( 'NONE',  ( -1.572563554680370679, -4.781424942684484591, 3.380172092915589843 ) ) ;
#7593 = CARTESIAN_POINT ( 'NONE',  ( 1.378221871957440170, -0.4201271186440679872, 6.607619368096269596 ) ) ;
#7594 = LINE ( 'NONE', #13245, #2300 ) ;
#7595 = VECTOR ( 'NONE', #7561, 1000.000000000000000 ) ;
#7596 = DIRECTION ( 'NONE',  ( -1.746418240983389920E-16, 1.000000000000000000, 0.000000000000000000 ) ) ;
#7597 = ORIENTED_EDGE ( 'NONE', *, *, #18146, .F. ) ;
#7598 = EDGE_CURVE ( 'NONE', #1106, #1943, #8792, .T. ) ;
#7599 = CARTESIAN_POINT ( 'NONE',  ( -1.795861365445549973, -0.2491525423728821742, 3.705232155007899930 ) ) ;
#7600 = CARTESIAN_POINT ( 'NONE',  ( -1.465095039565370127, -3.566593075333519991, 2.858195935359880480 ) ) ;
#7601 = ORIENTED_EDGE ( 'NONE', *, *, #2102, .T. ) ;
#7602 = VERTEX_POINT ( 'NONE', #193 ) ;
#7603 = DIRECTION ( 'NONE',  ( 0.9622640697945186172, -0.2721173643531222264, 0.000000000000000000 ) ) ;
#7604 = CIRCLE ( 'NONE', #13221, 0.6099999999999999867 ) ;
#7605 = ORIENTED_EDGE ( 'NONE', *, *, #10395, .F. ) ;
#7606 = VECTOR ( 'NONE', #1753, 1000.000000000000000 ) ;
#7607 = CARTESIAN_POINT ( 'NONE',  ( 0.1749999999999999889, 9.099999999999999645, 0.5999999999999999778 ) ) ;
#7608 = CONTEXT_DEPENDENT_SHAPE_REPRESENTATION ( #467, #16734 ) ;
#7609 = CARTESIAN_POINT ( 'NONE',  ( -2.601107615185130673, -5.215466101694915757, 5.226397344856384741 ) ) ;
#7610 = CARTESIAN_POINT ( 'NONE',  ( -2.500000000000000000, 7.299999999999999822, 1.600000000000000089 ) ) ;
#7611 = VECTOR ( 'NONE', #3713, 1000.000000000000000 ) ;
#7612 = LINE ( 'NONE', #16129, #14689 ) ;
#7613 = VECTOR ( 'NONE', #7355, 1000.000000000000000 ) ;
#7614 = ORIENTED_EDGE ( 'NONE', *, *, #8952, .F. ) ;
#7615 = AXIS2_PLACEMENT_3D ( 'NONE', #5070, #1538, #8921 ) ;
#7616 = LINE ( 'NONE', #1804, #13529 ) ;
#7617 = CARTESIAN_POINT ( 'NONE',  ( 1.058024172752470182, -3.869340823081269587, 2.940600473883339561 ) ) ;
#7618 = CARTESIAN_POINT ( 'NONE',  ( 2.230812463554230352, -0.1023305084745770588, 6.137473736419911674 ) ) ;
#7619 = VECTOR ( 'NONE', #13377, 1000.000000000000000 ) ;
#7620 = ORIENTED_EDGE ( 'NONE', *, *, #12760, .T. ) ;
#7621 = CARTESIAN_POINT ( 'NONE',  ( -1.899999999999999911, 8.500000000000000000, 0.6099999999999999867 ) ) ;
#7622 = CARTESIAN_POINT ( 'NONE',  ( -1.432215783582709401, -0.4868644067796619179, 6.170863372171116801 ) ) ;
#7623 = ORIENTED_EDGE ( 'NONE', *, *, #13902, .F. ) ;
#7624 = CARTESIAN_POINT ( 'NONE',  ( 0.08231150243515643339, -0.001483050847457899508, 2.050000000000001155 ) ) ;
#7625 = VERTEX_POINT ( 'NONE', #16950 ) ;
#7626 = VECTOR ( 'NONE', #9337, 1000.000000000000000 ) ;
#7627 = LINE ( 'NONE', #10398, #10306 ) ;
#7628 = CARTESIAN_POINT ( 'NONE',  ( 4.898587196589409994E-17, -6.000000000000000000, -3.673940397442060361E-16 ) ) ;
#7629 = VECTOR ( 'NONE', #14722, 1000.000000000000000 ) ;
#7630 = CARTESIAN_POINT ( 'NONE',  ( 1.899999999999999911, 0.8000000000000000444, -1.674850734291659957E-15 ) ) ;
#7631 = CIRCLE ( 'NONE', #17048, 0.1499999999999999667 ) ;
#7632 = CARTESIAN_POINT ( 'NONE',  ( 1.370891210199511434, -3.869340823081269587, 2.427606771969341715 ) ) ;
#7633 = ORIENTED_EDGE ( 'NONE', *, *, #7669, .T. ) ;
#7634 = AXIS2_PLACEMENT_3D ( 'NONE', #8006, #13829, #9655 ) ;
#7635 = CARTESIAN_POINT ( 'NONE',  ( -1.687170344131989852, -2.848497014756560475, 6.340793075730589479 ) ) ;
#7636 = CARTESIAN_POINT ( 'NONE',  ( -0.02999999999999939868, 11.40000000000000036, 1.600000000000000089 ) ) ;
#7637 = VECTOR ( 'NONE', #16186, 1000.000000000000114 ) ;
#7638 = CARTESIAN_POINT ( 'NONE',  ( 1.491388273269019571, -4.012911429170968880, 6.110908523251506352 ) ) ;
#7639 = PRESENTATION_LAYER_ASSIGNMENT (  '', '', ( #6157 ) ) ;
#7640 = CARTESIAN_POINT ( 'NONE',  ( -1.899999999999999911, 11.40000000000000036, 7.550000000000000711 ) ) ;
#7641 = CARTESIAN_POINT ( 'NONE',  ( -1.971820545011380821, -1.544352870612421880, 4.128313389260230615 ) ) ;
#7642 = VERTEX_POINT ( 'NONE', #15306 ) ;
#7643 = EDGE_CURVE ( 'NONE', #11239, #11698, #12644, .T. ) ;
#7644 = CARTESIAN_POINT ( 'NONE',  ( 1.526064881623949931, -0.7763906680874419486, 2.903976516638540062 ) ) ;
#7645 = CARTESIAN_POINT ( 'NONE',  ( 2.573461662271340877, -0.7525510688106187285, 5.348389362822485893 ) ) ;
#7646 = ORIENTED_EDGE ( 'NONE', *, *, #5156, .T. ) ;
#7647 = CARTESIAN_POINT ( 'NONE',  ( -1.899999999999999911, 7.299999999999999822, 1.600000000000000089 ) ) ;
#7648 = LINE ( 'NONE', #13198, #15163 ) ;
#7649 = LINE ( 'NONE', #16000, #6817 ) ;
#7650 = CARTESIAN_POINT ( 'NONE',  ( -1.428515267734880023, -5.268855932203390324, 2.829745655876930055 ) ) ;
#7651 = ORIENTED_EDGE ( 'NONE', *, *, #10288, .T. ) ;
#7652 = VERTEX_POINT ( 'NONE', #14074 ) ;
#7653 = CARTESIAN_POINT ( 'NONE',  ( 2.350000000000000089, -6.000000000000000000, 2.799999999999999822 ) ) ;
#7654 = DIRECTION ( 'NONE',  ( -1.224646799147350002E-16, 1.000000000000000000, 6.123233995736769734E-17 ) ) ;
#7655 = AXIS2_PLACEMENT_3D ( 'NONE', #9520, #15178, #2487 ) ;
#7656 = DIRECTION ( 'NONE',  ( 2.986159789035700404E-15, -1.110223024625159992E-16, -1.000000000000000000 ) ) ;
#7657 = ORIENTED_EDGE ( 'NONE', *, *, #11407, .T. ) ;
#7658 = FACE_OUTER_BOUND ( 'NONE', #13158, .T. ) ;
#7659 = CARTESIAN_POINT ( 'NONE',  ( -0.7137241095604881513, -2.099430913171361102, 2.143887406933340678 ) ) ;
#7660 = EDGE_CURVE ( 'NONE', #10817, #14318, #2710, .T. ) ;
#7661 = FACE_OUTER_BOUND ( 'NONE', #5996, .T. ) ;
#7662 = LINE ( 'NONE', #17540, #18240 ) ;
#7663 = CARTESIAN_POINT ( 'NONE',  ( -2.023259452208839626, -3.174533050792599731, 3.497849062500260064 ) ) ;
#7664 = ADVANCED_FACE ( 'NONE', ( #11119 ), #5576, .T. ) ;
#7665 = CARTESIAN_POINT ( 'NONE',  ( 0.009452110982655383825, -5.000192044704546035, 2.050000000000001155 ) ) ;
#7666 = CARTESIAN_POINT ( 'NONE',  ( -2.281778813005780115, -4.847448931189379806, 5.276394947932169899 ) ) ;
#7667 = EDGE_CURVE ( 'NONE', #14593, #6821, #7237, .T. ) ;
#7668 = VECTOR ( 'NONE', #15394, 1000.000000000000000 ) ;
#7669 = EDGE_CURVE ( 'NONE', #13769, #2785, #1224, .T. ) ;
#7670 = CARTESIAN_POINT ( 'NONE',  ( 1.508881462028659692, -4.311818300558746486, 6.092184821126257255 ) ) ;
#7671 = DIRECTION ( 'NONE',  ( 1.036208156316810036E-14, 1.000000000000000000, 0.000000000000000000 ) ) ;
#7672 = DIRECTION ( 'NONE',  ( -1.000000000000000000, 0.000000000000000000, 0.000000000000000000 ) ) ;
#7673 = CARTESIAN_POINT ( 'NONE',  ( -1.057242234132100167, -5.577754237288139905, 2.597442975781530272 ) ) ;
#7674 = ORIENTED_EDGE ( 'NONE', *, *, #322, .T. ) ;
#7675 = CARTESIAN_POINT ( 'NONE',  ( 1.534924416212170017, -5.333856471232000018, 2.911460733964629899 ) ) ;
#7676 = ORIENTED_EDGE ( 'NONE', *, *, #8407, .T. ) ;
#7677 = LINE ( 'NONE', #7859, #7889 ) ;
#7678 = CARTESIAN_POINT ( 'NONE',  ( -0.4000000000000000222, -1.399999999999999911, 5.100000000000000533 ) ) ;
#7679 = VERTEX_POINT ( 'NONE', #18128 ) ;
#7680 = AXIS2_PLACEMENT_3D ( 'NONE', #11752, #3395, #8964 ) ;
#7681 = CARTESIAN_POINT ( 'NONE',  ( -2.111627294540180166, -1.889836318576769925, 3.660877362176710559 ) ) ;
#7682 = EDGE_CURVE ( 'NONE', #14961, #8260, #16766, .T. ) ;
#7683 = CARTESIAN_POINT ( 'NONE',  ( -1.899999999999999911, 11.29999999999999893, 7.649999999999999467 ) ) ;
#7684 = PLANE ( 'NONE',  #5827 ) ;
#7685 = DIRECTION ( 'NONE',  ( 1.000000000000000000, -1.762990951820104838E-17, 2.220446049250309876E-16 ) ) ;
#7686 = ADVANCED_FACE ( 'NONE', ( #13989 ), #12602, .T. ) ;
#7687 = CARTESIAN_POINT ( 'NONE',  ( 2.329383452786330189, -1.028169651910100013, 5.035735636132829818 ) ) ;
#7688 = CARTESIAN_POINT ( 'NONE',  ( 2.192143888961729736, -4.218665147405599392, 5.556300681753580051 ) ) ;
#7689 = CARTESIAN_POINT ( 'NONE',  ( 1.903446074666960364, -3.919758276017824006, 5.469282057156545029 ) ) ;
#7690 = CARTESIAN_POINT ( 'NONE',  ( -1.000000000000000000, -5.599999999999999645, 3.673738709727309981 ) ) ;
#7691 = CIRCLE ( 'NONE', #9470, 0.04999999999999969746 ) ;
#7692 = CARTESIAN_POINT ( 'NONE',  ( 1.899999999999999911, 11.40000000000000036, 7.599999999999999645 ) ) ;
#7693 = EDGE_LOOP ( 'NONE', ( #12595, #66, #9346, #13675 ) ) ;
#7694 = CARTESIAN_POINT ( 'NONE',  ( 1.575321925694149972, -5.277599664614070818, 3.124678074305839992 ) ) ;
#7695 = CARTESIAN_POINT ( 'NONE',  ( 1.246151616534670215, -0.3311440677966111523, 3.068501529594759081 ) ) ;
#7696 = CARTESIAN_POINT ( 'NONE',  ( -1.816660071039029933, -3.170692174432619748, 6.196159040268240936 ) ) ;
#7697 = ORIENTED_EDGE ( 'NONE', *, *, #12212, .F. ) ;
#7698 = VERTEX_POINT ( 'NONE', #5756 ) ;
#7699 = DIRECTION ( 'NONE',  ( 0.000000000000000000, 0.000000000000000000, 1.000000000000000000 ) ) ;
#7700 = ORIENTED_EDGE ( 'NONE', *, *, #11971, .F. ) ;
#7701 = LINE ( 'NONE', #949, #17456 ) ;
#7702 = ITEM_DEFINED_TRANSFORMATION ( 'NONE', 'NONE', #4400,  #17681 ) ;
#7703 = CARTESIAN_POINT ( 'NONE',  ( -1.000896394980330006, -5.170974576271190948, 6.829956240957379521 ) ) ;
#7704 = PRODUCT ( 'Insulating Base Plate', 'Insulating Base Plate', '', ( #1613 ) ) ;
#7705 = DIRECTION ( 'NONE',  ( 0.000000000000000000, 0.000000000000000000, -1.000000000000000000 ) ) ;
#7706 = VECTOR ( 'NONE', #17810, 1000.000000000000000 ) ;
#7707 = LINE ( 'NONE', #14737, #5532 ) ;
#7708 = ORIENTED_EDGE ( 'NONE', *, *, #15065, .T. ) ;
#7709 = ADVANCED_FACE ( 'NONE', ( #17203 ), #6102, .F. ) ;
#7710 = CARTESIAN_POINT ( 'NONE',  ( 1.889999999999999902, 4.700000000000000178, -5.846397852431180656E-16 ) ) ;
#7711 = CARTESIAN_POINT ( 'NONE',  ( 0.7205524543785531977, -4.428259742000194343, 6.622421910798232503 ) ) ;
#7712 = CARTESIAN_POINT ( 'NONE',  ( -0.07064654565474801085, -0.4512711864406789841, 7.352897294663512717 ) ) ;
#7713 =( BOUNDED_SURFACE ( )  B_SPLINE_SURFACE ( 3, 3, ( 
 ( #9259, #2228, #17850, #9546, #7875, #5095, #10747 ),
 ( #12325, #16394, #13629, #16586, #9345, #12232, #939 ),
 ( #8158, #15016, #5383, #13799, #13716, #18039, #5189 ),
 ( #2334, #10838, #1123, #3978, #16486, #2606, #8255 ),
 ( #3803, #2431, #8076, #4247, #1211, #18119, #9910 ),
 ( #4437, #11301, #14066, #14176, #15566, #16754, #5829 ),
 ( #1388, #16938, #4071, #7054, #7151, #2786, #18209 ) ),
 .UNSPECIFIED., .T., .F., .F. ) 
 B_SPLINE_SURFACE_WITH_KNOTS ( ( 4, 3, 4 ),
 ( 4, 1, 1, 1, 4 ),
 ( 0.000000000000000000, 3.141592653589790007, 6.283185307179590673 ),
 ( 5.497787143782139729, 5.798117950472390092, 5.930336460519450625, 6.055422062302069364, 6.283185307179590673 ),
 .UNSPECIFIED. ) 
 GEOMETRIC_REPRESENTATION_ITEM ( )  RATIONAL_B_SPLINE_SURFACE ( (
 ( 1.000000000000000000, 1.000000000000000000, 1.000000000000000000, 1.000000000000000000, 1.000000000000000000, 1.000000000000000000, 1.000000000000000000),
 ( 0.3333333333333329818, 0.3333333333333329818, 0.3333333333333329818, 0.3333333333333329818, 0.3333333333333329818, 0.3333333333333329818, 0.3333333333333329818),
 ( 0.3333333333333329818, 0.3333333333333329818, 0.3333333333333329818, 0.3333333333333329818, 0.3333333333333329818, 0.3333333333333329818, 0.3333333333333329818),
 ( 1.000000000000000000, 1.000000000000000000, 1.000000000000000000, 1.000000000000000000, 1.000000000000000000, 1.000000000000000000, 1.000000000000000000),
 ( 0.3333333333333329818, 0.3333333333333329818, 0.3333333333333329818, 0.3333333333333329818, 0.3333333333333329818, 0.3333333333333329818, 0.3333333333333329818),
 ( 0.3333333333333329818, 0.3333333333333329818, 0.3333333333333329818, 0.3333333333333329818, 0.3333333333333329818, 0.3333333333333329818, 0.3333333333333329818),
 ( 1.000000000000000000, 1.000000000000000000, 1.000000000000000000, 1.000000000000000000, 1.000000000000000000, 1.000000000000000000, 1.000000000000000000) ) ) 
 REPRESENTATION_ITEM ( '' )  SURFACE ( )  );
#7714 = ORIENTED_EDGE ( 'NONE', *, *, #4777, .T. ) ;
#7715 = CARTESIAN_POINT ( 'NONE',  ( -1.289141334274979789, -0.4824152542372879826, 6.297747079672432413 ) ) ;
#7716 = CARTESIAN_POINT ( 'NONE',  ( 2.484260633728970546, -0.05783898305084796132, 3.766563288620793593 ) ) ;
#7717 = ORIENTED_EDGE ( 'NONE', *, *, #15478, .F. ) ;
#7718 = CIRCLE ( 'NONE', #3880, 0.1999999999999999833 ) ;
#7719 = CARTESIAN_POINT ( 'NONE',  ( -1.596341326794979976, -5.564406779661021041, 2.970780074643819990 ) ) ;
#7720 = CARTESIAN_POINT ( 'NONE',  ( 1.282210379528779809, -0.9388573751169242421, 6.673494927815259103 ) ) ;
#7721 = CARTESIAN_POINT ( 'NONE',  ( -0.8147348917079840769, -0.2831443699174389650, 2.488757019513870183 ) ) ;
#7722 = CARTESIAN_POINT ( 'NONE',  ( -2.295344368707641358, -3.473439922180372452, 3.367893426919611688 ) ) ;
#7723 = ORIENTED_EDGE ( 'NONE', *, *, #1236, .T. ) ;
#7724 = MANIFOLD_SOLID_BREP ( 'Stock-MAS-687-1', #10526 ) ;
#7725 = CARTESIAN_POINT ( 'NONE',  ( 1.741913176380120110, -3.640298816558360073, 3.117443785062520067 ) ) ;
#7726 = DIRECTION ( 'NONE',  ( -1.000000000000000000, 7.105427357601000281E-16, -1.776356839400249824E-16 ) ) ;
#7727 = LINE ( 'NONE', #14582, #14636 ) ;
#7728 = CARTESIAN_POINT ( 'NONE',  ( -1.538437905835030595, -3.221109627369172390, 3.340547664492051094 ) ) ;
#7729 = FACE_BOUND ( 'NONE', #16231, .T. ) ;
#7730 = DIRECTION ( 'NONE',  ( 0.000000000000000000, -1.000000000000000000, 9.633757521571540356E-31 ) ) ;
#7731 = CARTESIAN_POINT ( 'NONE',  ( -1.065036425887979421, -1.218316834576379737, 6.455163597548632559 ) ) ;
#7732 = ORIENTED_EDGE ( 'NONE', *, *, #2087, .T. ) ;
#7733 = LINE ( 'NONE', #2378, #3470 ) ;
#7734 = CARTESIAN_POINT ( 'NONE',  ( -0.1749999999999999889, 9.299999999999998934, 0.4000000000000000222 ) ) ;
#7735 = ORIENTED_EDGE ( 'NONE', *, *, #3579, .F. ) ;
#7736 = CYLINDRICAL_SURFACE ( 'NONE', #13523, 0.09999999999999986677 ) ;
#7737 = CARTESIAN_POINT ( 'NONE',  ( -6.735557395310440051E-17, 7.000000000000000000, 6.299999999999999822 ) ) ;
#7738 = DIRECTION ( 'NONE',  ( 0.000000000000000000, -1.000000000000000000, 0.000000000000000000 ) ) ;
#7739 = CARTESIAN_POINT ( 'NONE',  ( -2.203023580853999963, -5.242161016949149932, 3.872235369154300333 ) ) ;
#7740 = ORIENTED_EDGE ( 'NONE', *, *, #17579, .T. ) ;
#7741 = ORIENTED_EDGE ( 'NONE', *, *, #10610, .F. ) ;
#7742 = CARTESIAN_POINT ( 'NONE',  ( -1.889999999999999902, 7.900000000000000355, 3.000000000000000000 ) ) ;
#7743 = DIRECTION ( 'NONE',  ( 0.000000000000000000, 0.000000000000000000, -1.000000000000000000 ) ) ;
#7744 = CARTESIAN_POINT ( 'NONE',  ( 1.526064881623949931, -0.7763906680874419486, 2.903976516638540062 ) ) ;
#7745 = ADVANCED_BREP_SHAPE_REPRESENTATION ( '', ( #2155, #17681 ), #11500 ) ;
#7746 = ORIENTED_EDGE ( 'NONE', *, *, #9159, .F. ) ;
#7747 = CARTESIAN_POINT ( 'NONE',  ( 0.6187874668174475623, -5.435381355932195291, 6.657494107589526422 ) ) ;
#7748 = CARTESIAN_POINT ( 'NONE',  ( -2.146130664537640786, -3.197821339080880065, 3.138834773724098692 ) ) ;
#7749 = CARTESIAN_POINT ( 'NONE',  ( -0.3750000000000000000, 6.450000000000000178, 2.100000000000000089 ) ) ;
#7750 = CARTESIAN_POINT ( 'NONE',  ( -2.644456467089570939, -1.796683165423619055, 4.476474416072687035 ) ) ;
#7751 = AXIS2_PLACEMENT_3D ( 'NONE', #2326, #13623, #7975 ) ;
#7752 = CARTESIAN_POINT ( 'NONE',  ( -11.62823001646920140, 1.398466485101550089E-14, -4.396483177515619900E-14 ) ) ;
#7753 = DIRECTION ( 'NONE',  ( 0.000000000000000000, 0.000000000000000000, 1.000000000000000000 ) ) ;
#7754 = CARTESIAN_POINT ( 'NONE',  ( 1.710920205120059823, -4.012911429170970656, 6.316012914303540171 ) ) ;
#7755 = DIRECTION ( 'NONE',  ( 0.000000000000000000, 0.000000000000000000, -1.000000000000000000 ) ) ;
#7756 = CARTESIAN_POINT ( 'NONE',  ( -0.2335786437626909962, 3.050000000000000266, 2.241421356237310203 ) ) ;
#7758 = ORIENTED_EDGE ( 'NONE', *, *, #18053, .F. ) ;
#7757 = CARTESIAN_POINT ( 'NONE',  ( -0.8400312909772689185, -3.030962444702889780, 7.217431453521816920 ) ) ;
#7759 = LINE ( 'NONE', #13404, #6425 ) ;
#7760 = LINE ( 'NONE', #2489, #2631 ) ;
#7761 = CARTESIAN_POINT ( 'NONE',  ( 0.5000000000000000000, 5.762741699796949391, 5.100000000000000533 ) ) ;
#7762 = FACE_OUTER_BOUND ( 'NONE', #16292, .T. ) ;
#7763 = CARTESIAN_POINT ( 'NONE',  ( -2.308170020371289599, -1.726818300558750074, 5.159452766389659217 ) ) ;
#7764 = CARTESIAN_POINT ( 'NONE',  ( -1.250000000000000000, 3.881370849898470254, 6.100000000000000533 ) ) ;
#7765 = CARTESIAN_POINT ( 'NONE',  ( 2.020286629067969297, -5.408686440677975327, 6.420841923842827370 ) ) ;
#7766 = ORIENTED_EDGE ( 'NONE', *, *, #10051, .T. ) ;
#7767 = CARTESIAN_POINT ( 'NONE',  ( 1.972152263052529951E-31, 9.299999999999998934, 5.100000000000000533 ) ) ;
#7768 = DIRECTION ( 'NONE',  ( -1.000000000000000000, 0.000000000000000000, 6.123233995736769734E-17 ) ) ;
#7769 = DIRECTION ( 'NONE',  ( -1.000000000000000000, 2.220446049250309876E-16, 0.000000000000000000 ) ) ;
#7770 = EDGE_CURVE ( 'NONE', #13022, #10426, #8973, .T. ) ;
#7771 = ORIENTED_EDGE ( 'NONE', *, *, #12318, .F. ) ;
#7772 = EDGE_CURVE ( 'NONE', #13357, #10192, #3064, .T. ) ;
#7773 = VERTEX_POINT ( 'NONE', #3328 ) ;
#7774 = CARTESIAN_POINT ( 'NONE',  ( 1.353103843060669886, -2.798079561820010053, 6.625579309552930063 ) ) ;
#7775 = LINE ( 'NONE', #15195, #17081 ) ;
#7776 = CARTESIAN_POINT ( 'NONE',  ( 1.641808337277750107, -5.413135593220339103, 6.386111670537619744 ) ) ;
#7777 = CARTESIAN_POINT ( 'NONE',  ( 0.2818998297622880012, -1.354205687946139935, 7.036509827384409554 ) ) ;
#7778 = CARTESIAN_POINT ( 'NONE',  ( 1.928470600873580132, -2.472043525783979678, 3.995796205495612874 ) ) ;
#7779 = CARTESIAN_POINT ( 'NONE',  ( 1.800000000000000044, 0.5999999999999999778, 1.600000000000000089 ) ) ;
#7780 = CARTESIAN_POINT ( 'NONE',  ( 0.2189795514005130062, -0.3044491525423729805, 2.356806637999009801 ) ) ;
#7781 = DIRECTION ( 'NONE',  ( -4.810966440042350793E-15, 0.000000000000000000, -1.000000000000000000 ) ) ;
#7782 = ORIENTED_EDGE ( 'NONE', *, *, #11308, .T. ) ;
#7783 = CARTESIAN_POINT ( 'NONE',  ( 1.699999999999999956, 2.299999999999999822, 7.599999999999999645 ) ) ;
#7784 = LINE ( 'NONE', #1033, #14618 ) ;
#7785 = MANIFOLD_SOLID_BREP ( 'Stock-MAS-687-1', #17327 ) ;
#7786 = CARTESIAN_POINT ( 'NONE',  ( -1.917298190932639868, -3.496728210468659892, 3.335187436117939885 ) ) ;
#7787 = VERTEX_POINT ( 'NONE', #7326 ) ;
#7788 = ORIENTED_EDGE ( 'NONE', *, *, #5769, .F. ) ;
#7789 = DIRECTION ( 'NONE',  ( -0.7071067811865480168, 0.000000000000000000, 0.7071067811865470176 ) ) ;
#7790 = ADVANCED_FACE ( 'NONE', ( #12970 ), #557, .T. ) ;
#7791 = VERTEX_POINT ( 'NONE', #11858 ) ;
#7792 = LINE ( 'NONE', #9073, #1525 ) ;
#7793 = EDGE_CURVE ( 'NONE', #1785, #10043, #10004, .T. ) ;
#7794 = APPLICATION_PROTOCOL_DEFINITION ( 'draft international standard', 'automotive_design', 1998, #14650 ) ;
#7795 = CARTESIAN_POINT ( 'NONE',  ( -0.3743405594629430344, -5.157627118644070308, 7.023440622744399953 ) ) ;
#7796 = DIRECTION ( 'NONE',  ( -3.652293603810800245E-15, -1.332267629550183904E-15, 1.000000000000000000 ) ) ;
#7797 = LINE ( 'NONE', #17776, #7296 ) ;
#7798 = APPLICATION_CONTEXT ( 'automotive_design' ) ;
#7799 = CARTESIAN_POINT ( 'NONE',  ( 0.1526488871098231337, -3.752899381639833720, 2.652660223633551251 ) ) ;
#7800 = CARTESIAN_POINT ( 'NONE',  ( 0.4917262214558945632, -0.008898305084746043966, 2.092115739186370948 ) ) ;
#7801 = ORIENTED_EDGE ( 'NONE', *, *, #12132, .F. ) ;
#7802 = CARTESIAN_POINT ( 'NONE',  ( 0.07299321914061039640, -0.3014830508474579673, 2.350000000000000089 ) ) ;
#7803 = ORIENTED_EDGE ( 'NONE', *, *, #5085, .T. ) ;
#7804 = CARTESIAN_POINT ( 'NONE',  ( 0.8570167067220200163, -0.01779661016949179997, 2.508190348879349774 ) ) ;
#7805 = ORIENTED_EDGE ( 'NONE', *, *, #17646, .T. ) ;
#7806 = DIRECTION ( 'NONE',  ( 0.7071067811865489050, 0.000000000000000000, 0.7071067811865460184 ) ) ;
#7807 = EDGE_CURVE ( 'NONE', #8002, #16159, #16108, .T. ) ;
#7808 = CARTESIAN_POINT ( 'NONE',  ( 1.899999999999999911, 2.000000000000000000, 1.600000000000000089 ) ) ;
#7809 = CARTESIAN_POINT ( 'NONE',  ( 1.477796163681079911, -5.417584745762709986, 6.531563725478140015 ) ) ;
#7810 = CARTESIAN_POINT ( 'NONE',  ( -2.328527996529179411, -5.033755237495684653, 3.426787111016392107 ) ) ;
#7811 = VERTEX_POINT ( 'NONE', #9052 ) ;
#7812 = CARTESIAN_POINT ( 'NONE',  ( -0.4058874503045720172, 7.799999999999999822, 6.100000000000000533 ) ) ;
#7813 = VECTOR ( 'NONE', #3520, 1000.000000000000000 ) ;
#7814 = CARTESIAN_POINT ( 'NONE',  ( -2.347833536521260367, -3.058091609351150097, 4.537447324629909851 ) ) ;
#7815 = CARTESIAN_POINT ( 'NONE',  ( 0.2041457401074358857, -4.498124606865046893, 7.346023093209487875 ) ) ;
#7816 = CARTESIAN_POINT ( 'NONE',  ( 2.500000000000000000, 11.29999999999999893, 1.600000000000000089 ) ) ;
#7817 = DIRECTION ( 'NONE',  ( 0.000000000000000000, -1.000000000000000000, 1.110223024625159992E-16 ) ) ;
#7818 = CARTESIAN_POINT ( 'NONE',  ( -1.259207372045990869, -3.267686203945749490, 3.078488779929933639 ) ) ;
#7819 = CARTESIAN_POINT ( 'NONE',  ( 1.850000000000000089, 0.7500000000000000000, 7.700000000000000178 ) ) ;
#7820 = LINE ( 'NONE', #3552, #8839 ) ;
#7821 = ADVANCED_FACE ( 'NONE', ( #14709 ), #2503, .T. ) ;
#7822 = CARTESIAN_POINT ( 'NONE',  ( -1.372465729645771182, -1.264893411152960834, 6.226839763556076157 ) ) ;
#7823 = ORIENTED_EDGE ( 'NONE', *, *, #510, .F. ) ;
#7824 = DIRECTION ( 'NONE',  ( -0.7071067811865500152, 0.000000000000000000, -0.7071067811865451302 ) ) ;
#7825 = CARTESIAN_POINT ( 'NONE',  ( -1.899999999999999911, 10.00000000000000000, 1.600000000000000089 ) ) ;
#7826 = CARTESIAN_POINT ( 'NONE',  ( -2.398725280367459245, -3.151244762504313179, 3.564557036955213754 ) ) ;
#7827 = ORIENTED_EDGE ( 'NONE', *, *, #6435, .F. ) ;
#7828 = CARTESIAN_POINT ( 'NONE',  ( -0.5500000000000000444, 6.450000000000000178, 1.600000000000000089 ) ) ;
#7829 = CARTESIAN_POINT ( 'NONE',  ( 2.351212046067109984, -0.9815930753335269099, 4.597298481426010497 ) ) ;
#7830 = DIRECTION ( 'NONE',  ( -6.123233995736769734E-17, 3.749399456654650178E-33, -1.000000000000000000 ) ) ;
#7831 = CARTESIAN_POINT ( 'NONE',  ( 2.050059171113549183, -5.077542372881359789, 4.809263467226075228 ) ) ;
#7832 = ORIENTED_EDGE ( 'NONE', *, *, #18074, .F. ) ;
#7833 = EDGE_CURVE ( 'NONE', #240, #14839, #7775, .T. ) ;
#7834 = EDGE_LOOP ( 'NONE', ( #16130, #9851, #2184, #10333 ) ) ;
#7835 = DIRECTION ( 'NONE',  ( 1.000000000000000000, 0.000000000000000000, 0.000000000000000000 ) ) ;
#7836 = FACE_OUTER_BOUND ( 'NONE', #17951, .T. ) ;
#7837 = CARTESIAN_POINT ( 'NONE',  ( -0.1749999999999999889, 5.000000000000000000, 1.071565949253929989E-17 ) ) ;
#7838 = ORIENTED_EDGE ( 'NONE', *, *, #16735, .F. ) ;
#7839 = CARTESIAN_POINT ( 'NONE',  ( -1.088937603231280304, -5.573305084745765470, 2.959627624143549074 ) ) ;
#7840 = CARTESIAN_POINT ( 'NONE',  ( 1.597383073937500786, -3.593722239981783861, 2.580688553303249755 ) ) ;
#7841 = CARTESIAN_POINT ( 'NONE',  ( 1.661700935665417544, -5.037501140877957084, 3.038299064334577082 ) ) ;
#7842 = CARTESIAN_POINT ( 'NONE',  ( -2.639965200365840037, -1.750106588847040845, 4.971472712918284742 ) ) ;
#7843 = LINE ( 'NONE', #593, #15032 ) ;
#7844 = DIRECTION ( 'NONE',  ( -3.700743415417179758E-16, -1.000000000000000000, 0.000000000000000000 ) ) ;
#7845 = CARTESIAN_POINT ( 'NONE',  ( -0.9170541073686521161, -4.315659176918719808, 6.867431071947200039 ) ) ;
#7846 = LINE ( 'NONE', #4971, #3165 ) ;
#7847 = CARTESIAN_POINT ( 'NONE',  ( -0.6207106781186559896, 6.450000000000000178, 2.628553390593269423 ) ) ;
#7849 = VERTEX_POINT ( 'NONE', #2220 ) ;
#7848 = CARTESIAN_POINT ( 'NONE',  ( -1.700860513939528751, -3.124115597856051085, 6.737200825918551850 ) ) ;
#7850 = CARTESIAN_POINT ( 'NONE',  ( 0.1749999999999999889, 7.799999999999999822, 0.4000000000000000222 ) ) ;
#7851 = DIRECTION ( 'NONE',  ( -9.349246523159200620E-16, 0.000000000000000000, 1.000000000000000000 ) ) ;
#7852 = CARTESIAN_POINT ( 'NONE',  ( 0.7109160811436110450, -1.307629111369560171, 6.943511536198400336 ) ) ;
#7853 = CARTESIAN_POINT ( 'NONE',  ( -2.332582362116870200, -0.5313559322033900578, 4.387643303570819775 ) ) ;
#7854 = DIRECTION ( 'NONE',  ( 0.000000000000000000, 0.000000000000000000, 1.000000000000000000 ) ) ;
#7855 = CARTESIAN_POINT ( 'NONE',  ( 1.467041701146838406, -5.422033898305085309, 6.911479965439912831 ) ) ;
#7856 = ORIENTED_EDGE ( 'NONE', *, *, #13908, .F. ) ;
#7857 = DIRECTION ( 'NONE',  ( 1.531342102931250010E-16, -1.000000000000000000, 0.000000000000000000 ) ) ;
#7858 = CARTESIAN_POINT ( 'NONE',  ( 0.06264882350516236265, -5.148728813559319661, 7.052569299041217654 ) ) ;
#7859 = CARTESIAN_POINT ( 'NONE',  ( -0.5500000000000000444, 0.5999999999999999778, 1.600000000000000089 ) ) ;
#7860 = CARTESIAN_POINT ( 'NONE',  ( -1.600000000000000089, -9.269168731236250681E-17, 7.649999999999999467 ) ) ;
#7861 = AXIS2_PLACEMENT_3D ( 'NONE', #2536, #2260, #13836 ) ;
#7862 = EDGE_LOOP ( 'NONE', ( #16376, #9773, #15858, #1808, #10811, #9041 ) ) ;
#7863 = ORIENTED_EDGE ( 'NONE', *, *, #11714, .T. ) ;
#7864 = EDGE_CURVE ( 'NONE', #5954, #16609, #16579, .T. ) ;
#7865 = CARTESIAN_POINT ( 'NONE',  ( 1.902324933209389890, -2.402178660919109809, 3.314393441133530072 ) ) ;
#7866 = CARTESIAN_POINT ( 'NONE',  ( -1.978267656359410154, -5.497669491525420504, 5.974740860598790171 ) ) ;
#7867 = LINE ( 'NONE', #837, #12312 ) ;
#7868 = AXIS2_PLACEMENT_3D ( 'NONE', #8274, #10674, #2242 ) ;
#7869 = CARTESIAN_POINT ( 'NONE',  ( 2.276802572547980130, -2.495331814072260013, 4.104251954998760610 ) ) ;
#7870 = CARTESIAN_POINT ( 'NONE',  ( -6.735557395310420329E-17, 6.700000000000000178, 6.299999999999999822 ) ) ;
#7871 = CARTESIAN_POINT ( 'NONE',  ( 0.05638445020230590382, -1.377493976234431372, 6.752248190741917178 ) ) ;
#7872 = VECTOR ( 'NONE', #6181, 1000.000000000000000 ) ;
#7873 = DIRECTION ( 'NONE',  ( 6.123233995736767268E-17, -1.000000000000000000, 0.000000000000000000 ) ) ;
#7874 = ADVANCED_FACE ( 'NONE', ( #13419 ), #11940, .F. ) ;
#7875 = CARTESIAN_POINT ( 'NONE',  ( -0.4617942143426889690, -0.5906145504024210569, 2.383143958488499692 ) ) ;
#7876 = ORIENTED_EDGE ( 'NONE', *, *, #16540, .T. ) ;
#7877 = CARTESIAN_POINT ( 'NONE',  ( 1.600938225939040116, -5.062364510889980629, 3.099061774060949848 ) ) ;
#7878 = CARTESIAN_POINT ( 'NONE',  ( -2.500000000000000000, 11.15000000000000036, 8.358214404180679581E-16 ) ) ;
#7879 = CARTESIAN_POINT ( 'NONE',  ( 2.190084968185480374, -4.032358841099290103, 3.838447030292440054 ) ) ;
#7880 = EDGE_LOOP ( 'NONE', ( #17857, #5694, #16595, #16233 ) ) ;
#7881 = EDGE_LOOP ( 'NONE', ( #7582, #11503, #7255, #2389 ) ) ;
#7882 = DIRECTION ( 'NONE',  ( 0.000000000000000000, -7.930164461608259947E-17, 1.000000000000000000 ) ) ;
#7883 = EDGE_LOOP ( 'NONE', ( #571, #15095, #14612, #8643 ) ) ;
#7884 = FACE_OUTER_BOUND ( 'NONE', #17299, .T. ) ;
#7885 = CARTESIAN_POINT ( 'NONE',  ( -2.353194804772640314, -5.224364406779660186, 4.731327187377240229 ) ) ;
#7886 = VECTOR ( 'NONE', #16427, 1000.000000000000000 ) ;
#7887 = AXIS2_PLACEMENT_3D ( 'NONE', #17960, #3902, #12431 ) ;
#7888 = CIRCLE ( 'NONE', #18204, 0.4000000000000000222 ) ;
#7889 = VECTOR ( 'NONE', #550, 1000.000000000000000 ) ;
#7890 = VERTEX_POINT ( 'NONE', #642 ) ;
#7891 = CARTESIAN_POINT ( 'NONE',  ( 2.281778813005790330, -0.7525510688106179513, 5.276394947932120161 ) ) ;
#7892 = ADVANCED_FACE ( 'NONE', ( #6368 ), #834, .F. ) ;
#7893 = CARTESIAN_POINT ( 'NONE',  ( 1.899999999999999911, 9.199999999999999289, 1.600000000000000089 ) ) ;
#7894 = CARTESIAN_POINT ( 'NONE',  ( -1.673492459604430938, -3.496728210468663889, 3.510746103527421891 ) ) ;
#7895 = VECTOR ( 'NONE', #4218, 1000.000000000000000 ) ;
#7896 = EDGE_CURVE ( 'NONE', #1884, #6712, #9447, .T. ) ;
#7897 = CARTESIAN_POINT ( 'NONE',  ( 1.248294325655350034, -0.02669491525423759934, 2.704938983774300088 ) ) ;
#7898 = ORIENTED_EDGE ( 'NONE', *, *, #2452, .T. ) ;
#7899 = CARTESIAN_POINT ( 'NONE',  ( 2.116444151961470066, -0.3533898305084750002, 3.670839500609349937 ) ) ;
#7900 = EDGE_CURVE ( 'NONE', #11111, #5685, #10650, .T. ) ;
#7901 = AXIS2_PLACEMENT_3D ( 'NONE', #18095, #5530, #15363 ) ;
#7902 = CARTESIAN_POINT ( 'NONE',  ( -2.630358833876468960, -0.2313559322033900412, 4.347767980622416317 ) ) ;
#7903 = VECTOR ( 'NONE', #15875, 1000.000000000000000 ) ;
#7904 = VERTEX_POINT ( 'NONE', #5087 ) ;
#7905 = CARTESIAN_POINT ( 'NONE',  ( -2.340070819011249803, -5.519915254237290014, 4.950151441910549899 ) ) ;
#7906 = CARTESIAN_POINT ( 'NONE',  ( 2.296954468777709923, -0.6361096273691759784, 4.187412587068651604 ) ) ;
#7907 = CARTESIAN_POINT ( 'NONE',  ( 1.300961508564179914, -5.422033898305079092, 6.661123742937279602 ) ) ;
#7908 = AXIS2_PLACEMENT_3D ( 'NONE', #4178, #8544, #12800 ) ;
#7909 = VECTOR ( 'NONE', #14376, 1000.000000000000000 ) ;
#7910 = VECTOR ( 'NONE', #10655, 1000.000000000000114 ) ;
#7911 = CARTESIAN_POINT ( 'NONE',  ( 2.632587027711251526, -0.6593979156574641953, 4.364441905910536157 ) ) ;
#7912 = VERTEX_POINT ( 'NONE', #10738 ) ;
#7913 = DIRECTION ( 'NONE',  ( 0.000000000000000000, 0.000000000000000000, 1.000000000000000000 ) ) ;
#7914 = CARTESIAN_POINT ( 'NONE',  ( -0.7109160811435620841, -4.292370888630429704, 6.943511536198419876 ) ) ;
#7915 = CARTESIAN_POINT ( 'NONE',  ( -2.328527996529179411, -5.033755237495684653, 3.426787111016392107 ) ) ;
#7916 = CIRCLE ( 'NONE', #1400, 0.09999999999999990841 ) ;
#7917 = EDGE_CURVE ( 'NONE', #6842, #16761, #16385, .T. ) ;
#7918 = DIRECTION ( 'NONE',  ( -2.537652627714639929E-16, -1.000000000000000000, 0.000000000000000000 ) ) ;
#7919 = CARTESIAN_POINT ( 'NONE',  ( -1.764143222953850065, -3.174533050792599731, 3.649904513135073802 ) ) ;
#7921 = EDGE_CURVE ( 'NONE', #13368, #3854, #14424, .T. ) ;
#7920 = DIRECTION ( 'NONE',  ( 0.000000000000000000, 0.000000000000000000, 1.000000000000000000 ) ) ;
#7922 = DIRECTION ( 'NONE',  ( 3.700743415417190309E-15, -6.579099405186109509E-16, 1.000000000000000000 ) ) ;
#7923 = CARTESIAN_POINT ( 'NONE',  ( -0.7205524543785096769, -1.171740257999810852, 6.622421910798247602 ) ) ;
#7924 = ORIENTED_EDGE ( 'NONE', *, *, #1240, .T. ) ;
#7925 = CARTESIAN_POINT ( 'NONE',  ( -1.850000000000000089, -5.599999999999999645, 2.299999999999999822 ) ) ;
#7926 = DIRECTION ( 'NONE',  ( 1.059690869644410208E-14, 1.000000000000000000, -1.041146930477340028E-32 ) ) ;
#7927 = AXIS2_PLACEMENT_3D ( 'NONE', #3142, #17476, #4796 ) ;
#7928 = EDGE_CURVE ( 'NONE', #8163, #6491, #2423, .T. ) ;
#7929 = VECTOR ( 'NONE', #10456, 1000.000000000000000 ) ;
#7930 = CARTESIAN_POINT ( 'NONE',  ( 0.2254033459420760055, -0.6247245358507570456, 2.348900562125120217 ) ) ;
#7931 = CARTESIAN_POINT ( 'NONE',  ( -0.3832714063288900630, -2.685478996738538626, 7.326064873930687504 ) ) ;
#7932 = ORIENTED_EDGE ( 'NONE', *, *, #6216, .T. ) ;
#7933 = CARTESIAN_POINT ( 'NONE',  ( 1.250000000000000000, 6.144112549695430303, 5.100000000000000533 ) ) ;
#7934 = DIRECTION ( 'NONE',  ( 0.000000000000000000, -1.000000000000000000, 0.000000000000000000 ) ) ;
#7935 = DIRECTION ( 'NONE',  ( 6.083413833562510128E-16, -1.647588903766459698E-16, 1.000000000000000000 ) ) ;
#7936 = CARTESIAN_POINT ( 'NONE',  ( 2.034805890357269220, -5.068644067796615360, 4.427518626519221456 ) ) ;
#7937 = EDGE_LOOP ( 'NONE', ( #10361, #3166, #6544, #8863 ) ) ;
#7938 = AXIS2_PLACEMENT_3D ( 'NONE', #5611, #1442, #57 ) ;
#7939 = VERTEX_POINT ( 'NONE', #1020 ) ;
#7940 = CARTESIAN_POINT ( 'NONE',  ( 2.500000000000000000, 10.00000000000000000, 1.600000000000000089 ) ) ;
#7941 = CARTESIAN_POINT ( 'NONE',  ( 1.875000000000000000, 11.25000000000000000, 7.700000000000000178 ) ) ;
#7942 = LINE ( 'NONE', #3755, #9978 ) ;
#7943 = ORIENTED_EDGE ( 'NONE', *, *, #7557, .F. ) ;
#7944 = CARTESIAN_POINT ( 'NONE',  ( 0.9150601050661639757, -5.430932203389830626, 6.868218666554230190 ) ) ;
#7945 = VECTOR ( 'NONE', #12513, 1000.000000000000000 ) ;
#7946 = VECTOR ( 'NONE', #3504, 1000.000000000000000 ) ;
#7947 = CARTESIAN_POINT ( 'NONE',  ( 2.612083973477990373, -3.780028546288090041, 4.230818789270793800 ) ) ;
#7948 = DIRECTION ( 'NONE',  ( 5.181040781584069903E-15, 1.000000000000000000, 0.000000000000000000 ) ) ;
#7949 = PLANE ( 'NONE',  #11172 ) ;
#7950 = CARTESIAN_POINT ( 'NONE',  ( 0.5999999999999999778, 11.40000000000000036, 7.599999999999999645 ) ) ;
#7951 = CARTESIAN_POINT ( 'NONE',  ( 1.003115764947319910, -4.106064582324129297, 6.828967930617570126 ) ) ;
#7953 = ADVANCED_FACE ( 'NONE', ( #931 ), #6570, .T. ) ;
#7952 = LINE ( 'NONE', #13599, #4618 ) ;
#7954 = AXIS2_PLACEMENT_3D ( 'NONE', #592, #5026, #11891 ) ;
#7955 = DIRECTION ( 'NONE',  ( 0.000000000000000000, -0.2588190451025180749, 0.9659258262890690894 ) ) ;
#7957 = VERTEX_POINT ( 'NONE', #8336 ) ;
#7956 = CARTESIAN_POINT ( 'NONE',  ( 0.9880847989278174204, -2.262448931189378509, 2.236912075639679198 ) ) ;
#7958 = CARTESIAN_POINT ( 'NONE',  ( -1.399999999999999911, -8.000000000000000000, 6.100000000000000533 ) ) ;
#7959 = CARTESIAN_POINT ( 'NONE',  ( 6.735557395310435121E-17, 3.581751045813930112, 8.250000000000000000 ) ) ;
#7960 = AXIS2_PLACEMENT_3D ( 'NONE', #11834, #17266, #8953 ) ;
#7961 = CARTESIAN_POINT ( 'NONE',  ( -2.267872052190610166, -1.843259742000189938, 4.071110468860649867 ) ) ;
#7962 = CARTESIAN_POINT ( 'NONE',  ( -2.143090896833110381, -0.5046610169491529962, 5.672454929438350391 ) ) ;
#7963 = VECTOR ( 'NONE', #1600, 1000.000000000000000 ) ;
#7964 = CARTESIAN_POINT ( 'NONE',  ( -0.5500000000000000444, 6.450000000000000178, 2.699264068711930253 ) ) ;
#7965 = ORIENTED_EDGE ( 'NONE', *, *, #2642, .F. ) ;
#7966 = FILL_AREA_STYLE ('',( #5169 ) ) ;
#7967 = ORIENTED_EDGE ( 'NONE', *, *, #16143, .T. ) ;
#7968 = LINE ( 'NONE', #1016, #1714 ) ;
#7969 = CARTESIAN_POINT ( 'NONE',  ( 0.001589539283866070029, -0.4248071483275199789, 2.499688892524300154 ) ) ;
#7970 = VERTEX_POINT ( 'NONE', #18196 ) ;
#7971 = CARTESIAN_POINT ( 'NONE',  ( 2.311987889326980294, -4.078935417675859654, 4.260161748947079552 ) ) ;
#7972 = DIRECTION ( 'NONE',  ( -9.588835100573269740E-31, 1.000000000000000000, 3.548581835996780230E-45 ) ) ;
#7973 = CARTESIAN_POINT ( 'NONE',  ( -2.318251751302029984, -5.533262711864409766, 4.294764266798999586 ) ) ;
#7974 = AXIS2_PLACEMENT_3D ( 'NONE', #11411, #14002, #9502 ) ;
#7975 = DIRECTION ( 'NONE',  ( 0.000000000000000000, 0.000000000000000000, 1.000000000000000000 ) ) ;
#7976 = CARTESIAN_POINT ( 'NONE',  ( 2.352760675243219968, -2.565196678937129882, 4.757121734156020132 ) ) ;
#7977 = DIRECTION ( 'NONE',  ( -1.000000000000000000, 1.903239470785979823E-16, 0.000000000000000000 ) ) ;
#7978 = CARTESIAN_POINT ( 'NONE',  ( 0.9361665894546294941, -2.285737219477670390, 2.872845392579769452 ) ) ;
#7979 = DIRECTION ( 'NONE',  ( 0.000000000000000000, -1.000000000000000000, 0.000000000000000000 ) ) ;
#7980 = DIRECTION ( 'NONE',  ( -1.000000000000000000, 0.000000000000000000, 0.000000000000000000 ) ) ;
#7981 = LINE ( 'NONE', #15294, #2952 ) ;
#7982 = ORIENTED_EDGE ( 'NONE', *, *, #187, .T. ) ;
#7983 = DIRECTION ( 'NONE',  ( -1.908195823574489776E-16, 1.000000000000000000, 0.000000000000000000 ) ) ;
#7984 = CARTESIAN_POINT ( 'NONE',  ( -0.4000000000000000222, 2.399999999999999911, 5.100000000000000533 ) ) ;
#7985 = MANIFOLD_SOLID_BREP ( 'Stock-MAS-687-1', #1085 ) ;
#7986 = DIRECTION ( 'NONE',  ( 0.7071067811865480168, 0.000000000000000000, -0.7071067811865470176 ) ) ;
#7987 = EDGE_LOOP ( 'NONE', ( #14576, #15668, #4093, #11981 ) ) ;
#7988 = AXIS2_PLACEMENT_3D ( 'NONE', #15101, #6560, #5269 ) ;
#7989 = ORIENTED_EDGE ( 'NONE', *, *, #18096, .T. ) ;
#7990 = CARTESIAN_POINT ( 'NONE',  ( 1.399999999999999911, -6.000000000000000000, 5.100000000000000533 ) ) ;
#7991 = ORIENTED_EDGE ( 'NONE', *, *, #11332, .T. ) ;
#7992 = CARTESIAN_POINT ( 'NONE',  ( -1.250000000000000000, 3.881370849898470254, 5.100000000000000533 ) ) ;
#7993 = CARTESIAN_POINT ( 'NONE',  ( -1.378221871957430178, -5.179872881355930048, 6.607619368096279366 ) ) ;
#7994 = DIRECTION ( 'NONE',  ( 1.306144734853129823E-16, -1.000000000000000000, 0.000000000000000000 ) ) ;
#7995 = LINE ( 'NONE', #12430, #8543 ) ;
#7996 = ORIENTED_EDGE ( 'NONE', *, *, #17471, .F. ) ;
#7997 = CARTESIAN_POINT ( 'NONE',  ( 2.334748642087659753, -0.6593979156574649725, 4.403867486184820379 ) ) ;
#7998 = CARTESIAN_POINT ( 'NONE',  ( 1.875000000000000000, 11.25000000000000000, 7.700000000000000178 ) ) ;
#7999 = VECTOR ( 'NONE', #9116, 1000.000000000000000 ) ;
#8000 = CARTESIAN_POINT ( 'NONE',  ( -1.741913176380149864, -1.959701183441629802, 3.117443785062560035 ) ) ;
#8001 = CARTESIAN_POINT ( 'NONE',  ( -0.5609751937345790473, -0.1601694915254239793, 7.293870047334757523 ) ) ;
#8002 = VERTEX_POINT ( 'NONE', #5459 ) ;
#8003 = CARTESIAN_POINT ( 'NONE',  ( 1.875000000000000000, 12.00000000000000000, 7.700000000000000178 ) ) ;
#8004 = CARTESIAN_POINT ( 'NONE',  ( 2.270487904532159984, -0.06228813559322070315, 4.080813552109670894 ) ) ;
#8005 = ORIENTED_EDGE ( 'NONE', *, *, #13471, .T. ) ;
#8006 = CARTESIAN_POINT ( 'NONE',  ( -1.850000000000000089, 0.7500000000000000000, 8.300000000000000711 ) ) ;
#8007 = CARTESIAN_POINT ( 'NONE',  ( -2.192143888961709308, -1.381334852594400031, 5.556300681753639559 ) ) ;
#8008 = VECTOR ( 'NONE', #8120, 1000.000000000000000 ) ;
#8009 = CARTESIAN_POINT ( 'NONE',  ( -0.7197963925281907205, -0.5829339996946386604, 2.774540890140321014 ) ) ;
#8010 = EDGE_CURVE ( 'NONE', #17654, #1785, #17363, .T. ) ;
#8011 = CARTESIAN_POINT ( 'NONE',  ( -2.632587027711260852, -4.940602084342534894, 4.364441905910590336 ) ) ;
#8012 = ORIENTED_EDGE ( 'NONE', *, *, #3431, .F. ) ;
#8013 = CARTESIAN_POINT ( 'NONE',  ( -0.1749999999999999889, 7.700000000000000178, 1.600000000000000089 ) ) ;
#8014 = MANIFOLD_SOLID_BREP ( 'Stock-MAS-687-1', #481 ) ;
#8015 = EDGE_CURVE ( 'NONE', #9909, #6712, #12581, .T. ) ;
#8016 = CARTESIAN_POINT ( 'NONE',  ( 1.588913656381999884, -0.5196681859277345605, 3.399901838171224266 ) ) ;
#8017 = EDGE_CURVE ( 'NONE', #6927, #1371, #1290, .T. ) ;
#8018 = CARTESIAN_POINT ( 'NONE',  ( -1.899999999999999911, 3.500000000000000000, 0.6099999999999999867 ) ) ;
#8019 = DIRECTION ( 'NONE',  ( 1.000000000000000000, -2.220446049250309876E-16, 0.000000000000000000 ) ) ;
#8020 = CARTESIAN_POINT ( 'NONE',  ( 0.2475374578675958726, -1.354205687946139491, 6.738044908627027318 ) ) ;
#8021 = PRODUCT ( 'Movable Sliding Contacts', 'Movable Sliding Contacts', '', ( #13442 ) ) ;
#8022 = CARTESIAN_POINT ( 'NONE',  ( -2.500000000000000000, 4.700000000000000178, 0.5999999999999999778 ) ) ;
#8023 = DIRECTION ( 'NONE',  ( -1.000000000000000000, 0.000000000000000000, 0.000000000000000000 ) ) ;
#8024 = CARTESIAN_POINT ( 'NONE',  ( -1.472933559740131626, -2.848497014756559143, 6.130163826706357177 ) ) ;
#8025 = ORIENTED_EDGE ( 'NONE', *, *, #13168, .F. ) ;
#8026 = CARTESIAN_POINT ( 'NONE',  ( -3.763524982345449879E-15, -5.450000000000000178, 2.350000000000000089 ) ) ;
#8027 = VECTOR ( 'NONE', #12154, 1000.000000000000000 ) ;
#8028 = DIRECTION ( 'NONE',  ( -3.172065784643300034E-16, 1.000000000000000000, 0.000000000000000000 ) ) ;
#8029 = CARTESIAN_POINT ( 'NONE',  ( 0.9930264841371569950, -0.4076464065212260235, 2.562902636367419884 ) ) ;
#8030 = CARTESIAN_POINT ( 'NONE',  ( -0.2010642693394331104, -1.847100618360169699, 2.053740970238008501 ) ) ;
#8031 = ORIENTED_EDGE ( 'NONE', *, *, #2940, .F. ) ;
#8032 = FACE_OUTER_BOUND ( 'NONE', #17099, .T. ) ;
#8033 = DIRECTION ( 'NONE',  ( 4.476422471267168520E-17, 0.6823182503600082605, 0.7310552682428719251 ) ) ;
#8034 = CARTESIAN_POINT ( 'NONE',  ( -0.6964468257805866980, -5.166525423728809407, 6.631228347243847132 ) ) ;
#8035 = ORIENTED_EDGE ( 'NONE', *, *, #12425, .F. ) ;
#8036 = ADVANCED_FACE ( 'NONE', ( #4327 ), #733, .T. ) ;
#8037 = ORIENTED_EDGE ( 'NONE', *, *, #7317, .F. ) ;
#8038 = CARTESIAN_POINT ( 'NONE',  ( -1.399999999999999911, -5.000000000000000000, 6.100000000000000533 ) ) ;
#8039 = FACE_OUTER_BOUND ( 'NONE', #9119, .T. ) ;
#8040 = CARTESIAN_POINT ( 'NONE',  ( 3.591599821218599745E-17, 3.615866958331932057, 7.736552763412146483 ) ) ;
#8041 = ADVANCED_FACE ( 'NONE', ( #7566 ), #11641, .F. ) ;
#8042 = ORIENTED_EDGE ( 'NONE', *, *, #11868, .T. ) ;
#8043 = CARTESIAN_POINT ( 'NONE',  ( 2.328217775191430139, -5.381991525423729605, 5.043379051721160522 ) ) ;
#8044 = ADVANCED_FACE ( 'NONE', ( #10244 ), #3313, .T. ) ;
#8045 = CARTESIAN_POINT ( 'NONE',  ( -1.668426559427188982, -4.385524041783587457, 6.763847501343006385 ) ) ;
#8046 = DIRECTION ( 'NONE',  ( 0.7071067811865489050, 0.000000000000000000, -0.7071067811865461294 ) ) ;
#8047 = CARTESIAN_POINT ( 'NONE',  ( -2.502804106625960756, -3.426863345603793576, 3.817341913956430410 ) ) ;
#8048 = CARTESIAN_POINT ( 'NONE',  ( -1.800000000000000044, 11.40000000000000036, 7.550000000000000711 ) ) ;
#8049 = CARTESIAN_POINT ( 'NONE',  ( 2.255259958075439997, -3.896469987729530349, 5.372717034855999607 ) ) ;
#8050 = LINE ( 'NONE', #17738, #11149 ) ;
#8051 = FACE_OUTER_BOUND ( 'NONE', #6525, .T. ) ;
#8053 = ORIENTED_EDGE ( 'NONE', *, *, #10379, .F. ) ;
#8052 = CARTESIAN_POINT ( 'NONE',  ( -0.1110902655589390137, -2.961097579838030569, 7.351560417169478612 ) ) ;
#8054 = DIRECTION ( 'NONE',  ( 0.000000000000000000, -8.881784197001250351E-16, 1.000000000000000000 ) ) ;
#8055 = DIRECTION ( 'NONE',  ( 0.000000000000000000, 0.000000000000000000, 1.000000000000000000 ) ) ;
#8056 = CARTESIAN_POINT ( 'NONE',  ( -1.197297565406129971, -1.517223705964160008, 6.726135293448209929 ) ) ;
#8057 = CARTESIAN_POINT ( 'NONE',  ( -1.112838723655040107, -0.4735169491525429986, 6.773667561836210105 ) ) ;
#8058 = LINE ( 'NONE', #4982, #6803 ) ;
#8059 = CARTESIAN_POINT ( 'NONE',  ( 2.630358833876468960, -5.368644067796615182, 4.347767980622404771 ) ) ;
#8060 = ORIENTED_EDGE ( 'NONE', *, *, #10369, .T. ) ;
#8061 = DIRECTION ( 'NONE',  ( -3.700743415417179758E-16, -1.000000000000000000, 0.000000000000000000 ) ) ;
#8062 = ORIENTED_EDGE ( 'NONE', *, *, #15584, .T. ) ;
#8063 = CARTESIAN_POINT ( 'NONE',  ( 2.350067830300900162, -5.077542372881358901, 4.825253242917691310 ) ) ;
#8064 = CARTESIAN_POINT ( 'NONE',  ( 0.5000000000000000000, 3.500000000000000000, 5.100000000000000533 ) ) ;
#8065 = CARTESIAN_POINT ( 'NONE',  ( -1.149999999999999911, 9.274118095489749081, 7.596592582628910684 ) ) ;
#8066 = EDGE_CURVE ( 'NONE', #14289, #2611, #11554, .T. ) ;
#8067 = ORIENTED_EDGE ( 'NONE', *, *, #3196, .T. ) ;
#8068 = B_SPLINE_CURVE_WITH_KNOTS ( 'NONE', 3,
 ( #7420, #3244, #461, #6281, #643, #14539, #8888, #17395, #6103, #11768, #10363, #16029, #3329, #3602, #13622, #5179, #9338, #13710, #7776, #10651, #3791, #16580, #6759, #17557, #4889, #12035, #2127, #932, #10537, #17757, #9448, #14911, #16201, #13420, #15110, #735, #2221, #7866, #6571, #13518, #10931, #5281, #6658, #835, #15007, #7973, #3885, #2504, #3509, #6477, #9153, #15196, #6369, #2424, #8070, #12137, #16297, #9250, #1111, #12225, #1021, #5088 ),
 .UNSPECIFIED., .F., .F.,
 ( 4, 1, 1, 1, 1, 1, 1, 1, 1, 1, 1, 1, 1, 1, 1, 1, 1, 1, 1, 1, 1, 1, 1, 1, 1, 1, 1, 1, 1, 1, 1, 1, 1, 1, 1, 1, 1, 1, 1, 1, 1, 1, 1, 1, 1, 1, 1, 1, 1, 1, 1, 1, 1, 1, 1, 1, 1, 1, 1, 4 ),
 ( 0.7853981633974479459, 0.8785809963429079827, 0.9717638292883680196, 1.064946662233830166, 1.158129495179289981, 1.251312328124750017, 1.344495161070210054, 1.437677994015669869, 1.530860826961129906, 1.624043659906589943, 1.717226492852049979, 1.810409325797509794, 1.903592158742969609, 1.996774991688429868, 2.089957824633889683, 2.183140657579349941, 2.276323490524809756, 2.369506323470270015, 2.462689156415730274, 2.555871989361190089, 2.649054822306649903, 2.742237655252109718, 2.835420488197569977, 2.928603321143030236, 3.021786154088490051, 3.114968987033949865, 3.208151819979410124, 3.301334652924869939, 3.394517485870330198, 3.487700318815790013, 3.580883151761249827, 3.674065984706710086, 3.767248817652169901, 3.860431650597620390, 3.953614483543079761, 4.046797316488540019, 4.139980149433999834, 4.233162982379460537, 4.326345815324920352, 4.419528648270380167, 4.512711481215839981, 4.605894314161299796, 4.699077147106760499, 4.792259980052219426, 4.885442812997680129, 4.978625645943139943, 5.071808478888599758, 5.164991311834059573, 5.258174144779520276, 5.351356977724980091, 5.444539810670439905, 5.537722643615899720, 5.630905476561360423, 5.724088309506820238, 5.817271142452280053, 5.910453975397739868, 6.003636808343199682, 6.096819641288659497, 6.190002474234119312, 6.283185307179590673 ),
 .UNSPECIFIED. ) ;
#8069 = CARTESIAN_POINT ( 'NONE',  ( 0.3949552299394610277, -3.776187669928119828, 2.379923265530350385 ) ) ;
#8070 = CARTESIAN_POINT ( 'NONE',  ( -1.248294325655370018, -5.573305084745760141, 2.704938983774309857 ) ) ;
#8071 = CARTESIAN_POINT ( 'NONE',  ( -0.1749999999999999889, 8.500000000000000000, -3.200000000000000178 ) ) ;
#8072 = CARTESIAN_POINT ( 'NONE',  ( -1.669205944673819886, -3.147403886144329643, 6.359065158982450505 ) ) ;
#8073 = CARTESIAN_POINT ( 'NONE',  ( -2.161802606005209793, -5.010466949207389220, 3.769755311421840283 ) ) ;
#8074 = CARTESIAN_POINT ( 'NONE',  ( -1.385380178477320312, -1.982989471729918352, 3.184868453331453075 ) ) ;
#8075 = CARTESIAN_POINT ( 'NONE',  ( -1.899999999999999911, 4.700000000000000178, 0.5999999999999999778 ) ) ;
#8076 = CARTESIAN_POINT ( 'NONE',  ( -1.061361729696689515, -0.2742238837839081067, 2.926312958971010847 ) ) ;
#8077 = ORIENTED_EDGE ( 'NONE', *, *, #12674, .F. ) ;
#8078 = CARTESIAN_POINT ( 'NONE',  ( 1.300000000000000044, -1.592040838891560081E-16, 7.599999999999999645 ) ) ;
#8079 = CARTESIAN_POINT ( 'NONE',  ( -0.7999999999998790301, 11.40000000000000036, -2.399999999999999911 ) ) ;
#8080 = VERTEX_POINT ( 'NONE', #17267 ) ;
#8081 = ORIENTED_EDGE ( 'NONE', *, *, #17766, .T. ) ;
#8082 = UNCERTAINTY_MEASURE_WITH_UNIT (LENGTH_MEASURE( 1.000000000000000082E-05 ), #4521, 'distance_accuracy_value', 'NONE');
#8083 = ADVANCED_FACE ( 'NONE', ( #17186 ), #4508, .T. ) ;
#8084 = ORIENTED_EDGE ( 'NONE', *, *, #18074, .T. ) ;
#8085 = LINE ( 'NONE', #6778, #15720 ) ;
#8086 = CARTESIAN_POINT ( 'NONE',  ( -1.889104232906369862, -5.255508474576269684, 3.296507079072529933 ) ) ;
#8087 = CARTESIAN_POINT ( 'NONE',  ( -1.149999999999999911, 9.299999999999998934, 7.700000000000000178 ) ) ;
#8088 = CARTESIAN_POINT ( 'NONE',  ( -2.418933091173281369, -4.501965483225034426, 5.791730916219171021 ) ) ;
#8089 = CYLINDRICAL_SURFACE ( 'NONE', #4642, 0.6100000000000000977 ) ;
#8090 = CARTESIAN_POINT ( 'NONE',  ( 2.350542563031990273, -1.004881363621820123, 4.817027120179740329 ) ) ;
#8091 = CARTESIAN_POINT ( 'NONE',  ( 2.345900685764729765, -0.07118644067796649211, 4.512231114381330066 ) ) ;
#8092 = ORIENTED_EDGE ( 'NONE', *, *, #9115, .T. ) ;
#8093 = CARTESIAN_POINT ( 'NONE',  ( -2.286166334984490067, -0.5135593220338989795, 5.258525443163870605 ) ) ;
#8094 = ORIENTED_EDGE ( 'NONE', *, *, #7274, .T. ) ;
#8095 = CARTESIAN_POINT ( 'NONE',  ( 0.1765068388402390998, -0.1468220338983061424, 7.347961541693647902 ) ) ;
#8096 = VERTEX_POINT ( 'NONE', #4693 ) ;
#8097 = CARTESIAN_POINT ( 'NONE',  ( 1.899999999999999911, 0.5999999999999999778, 1.600000000000000089 ) ) ;
#8098 = CIRCLE ( 'NONE', #9869, 0.6500000000000003553 ) ;
#8099 = CARTESIAN_POINT ( 'NONE',  ( 1.820241257191439699, -0.5196681859277350046, 3.208199930689770163 ) ) ;
#8100 = CARTESIAN_POINT ( 'NONE',  ( -0.7983658734557950165, -5.466525423728810118, 6.913847129767330735 ) ) ;
#8101 = CARTESIAN_POINT ( 'NONE',  ( 2.622715975066190364, -0.7292627805223297344, 5.105554690682975405 ) ) ;
#8102 = VERTEX_POINT ( 'NONE', #15818 ) ;
#8103 = CARTESIAN_POINT ( 'NONE',  ( -0.4068869028847361125, -5.251463457376924104, 2.679545647941359743 ) ) ;
#8104 = CARTESIAN_POINT ( 'NONE',  ( -2.287919158821179799, -4.548542059801599535, 5.251517552016939483 ) ) ;
#8105 = EDGE_CURVE ( 'NONE', #14407, #7625, #533, .T. ) ;
#8106 = DIRECTION ( 'NONE',  ( 0.000000000000000000, 0.000000000000000000, -1.000000000000000000 ) ) ;
#8107 = DIRECTION ( 'NONE',  ( 0.000000000000000000, -1.000000000000000000, 0.000000000000000000 ) ) ;
#8108 = AXIS2_PLACEMENT_3D ( 'NONE', #1126, #6487, #942 ) ;
#8109 = CARTESIAN_POINT ( 'NONE',  ( 1.566607907718229553, -1.167899381639830203, 6.026891670824254810 ) ) ;
#8110 = DIRECTION ( 'NONE',  ( 1.000000000000000000, 5.551115123125880521E-15, -8.881784197001400629E-15 ) ) ;
#8111 = ORIENTED_EDGE ( 'NONE', *, *, #1546, .F. ) ;
#8112 = DIRECTION ( 'NONE',  ( 0.000000000000000000, 0.000000000000000000, 1.000000000000000000 ) ) ;
#8113 = DIRECTION ( 'NONE',  ( 1.224646799147350002E-16, -1.000000000000000000, -6.123233995736769734E-17 ) ) ;
#8114 = CARTESIAN_POINT ( 'NONE',  ( 1.622657008870240762E-16, -0.3000000000000002665, 2.649999999999998579 ) ) ;
#8115 = CARTESIAN_POINT ( 'NONE',  ( -0.6890111762203582346, -1.800524041783588824, 2.137115435286770282 ) ) ;
#8116 = CARTESIAN_POINT ( 'NONE',  ( 1.889999999999999902, 3.500000000000000000, 0.6099999999999999867 ) ) ;
#8117 = CARTESIAN_POINT ( 'NONE',  ( 1.399999999999999911, -5.500000000000000000, 6.100000000000000533 ) ) ;
#8118 = CARTESIAN_POINT ( 'NONE',  ( 1.940327948426050941, -5.390889830508485581, 5.370677689277660427 ) ) ;
#8119 = ORIENTED_EDGE ( 'NONE', *, *, #8960, .F. ) ;
#8120 = DIRECTION ( 'NONE',  ( -1.000000000000000000, 0.000000000000000000, 0.000000000000000000 ) ) ;
#8121 = VECTOR ( 'NONE', #7578, 1000.000000000000000 ) ;
#8122 = CARTESIAN_POINT ( 'NONE',  ( 2.328217775191430139, -5.381991525423729605, 5.043379051721160522 ) ) ;
#8123 = CARTESIAN_POINT ( 'NONE',  ( -1.000000000000000000, -5.599999999999999645, 5.100000000000000533 ) ) ;
#8124 = ORIENTED_EDGE ( 'NONE', *, *, #11516, .F. ) ;
#8125 = CARTESIAN_POINT ( 'NONE',  ( 2.058670345754650022, -5.350847457627120107, 3.559656372813920111 ) ) ;
#8126 = CARTESIAN_POINT ( 'NONE',  ( 0.9038768003982520227, -4.129352870612409632, 7.195219513931331967 ) ) ;
#8127 = B_SPLINE_CURVE_WITH_KNOTS ( 'NONE', 3,
 ( #18166, #4026, #9783, #7109, #14125, #8576, #2936, #4301, #16812, #7001, #5619, #1543, #145, #5432, #12556, #16714, #12831, #13947, #16988, #9963, #15444, #2753, #15628, #5794, #17074, #12650, #1263, #6908, #8396, #14033, #247, #11894, #13012, #1721, #10216, #6234, #3359, #5886, #10320, #3100, #8660, #1630, #3286, #14309, #7275, #3194, #13180, #10056, #12919, #11528, #17160, #15982, #15712, #11614, #8928, #17513, #15881, #17241, #4481, #496, #7373, #11807 ),
 .UNSPECIFIED., .F., .F.,
 ( 4, 1, 1, 1, 1, 1, 1, 1, 1, 1, 1, 1, 1, 1, 1, 1, 1, 1, 1, 1, 1, 1, 1, 1, 1, 1, 1, 1, 1, 1, 1, 1, 1, 1, 1, 1, 1, 1, 1, 1, 1, 1, 1, 1, 1, 1, 1, 1, 1, 1, 1, 1, 1, 1, 1, 1, 1, 1, 1, 4 ),
 ( 0.000000000000000000, 0.09318283294546000906, 0.1863656658909200181, 0.2795484988363799994, 0.3727313317818400362, 0.4659141647272999620, 0.5590969976727599988, 0.6522798306182200356, 0.7454626635636800724, 0.8386454965091399982, 0.9318283294545990358, 1.025011162400059961, 1.118193995345519998, 1.211376828290979812, 1.304559661236440071, 1.397742494181900108, 1.490925327127360145, 1.584108160072819960, 1.677290993018279996, 1.770473825963740033, 1.863656658909199848, 1.956839491854659885, 2.050022324800119922, 2.143205157745580181, 2.236387990691039995, 2.329570823636499810, 2.422753656581960069, 2.515936489527420328, 2.609119322472880143, 2.702302155418339957, 2.795484988363799772, 2.888667821309260031, 2.981850654254720290, 3.075033487200179660, 3.168216320145639919, 3.261399153091099734, 3.354581986036559993, 3.447764818982019808, 3.540947651927480067, 3.634130484872939437, 3.727313317818399696, 3.820496150763859955, 3.913678983709319770, 4.006861816654780029, 4.100044649600239843, 4.193227482545699658, 4.286410315491160361, 4.379593148436620176, 4.472775981382079991, 4.565958814327539805, 4.659141647272999620, 4.752324480218450553, 4.845507313163910368, 4.938690146109370183, 5.031872979054829997, 5.125055812000289812, 5.218238644945749627, 5.311421477891210330, 5.404604310836670145, 5.497787143782139729 ),
 .UNSPECIFIED. ) ;
#8128 = CARTESIAN_POINT ( 'NONE',  ( 0.9250303514740658706, -3.822764246504686270, 2.212544966868020602 ) ) ;
#8129 = LINE ( 'NONE', #3949, #3134 ) ;
#8130 = CARTESIAN_POINT ( 'NONE',  ( 1.588913656381999884, -0.5196681859277345605, 3.399901838171224266 ) ) ;
#8131 = DIRECTION ( 'NONE',  ( 1.000000000000000000, 1.283953296258166085E-32, -6.123233995736769734E-17 ) ) ;
#8132 = EDGE_CURVE ( 'NONE', #4379, #10381, #3223, .T. ) ;
#8133 = CARTESIAN_POINT ( 'NONE',  ( 1.500000000000000000, -6.000000000000000000, 2.299999999999999822 ) ) ;
#8134 = EDGE_CURVE ( 'NONE', #5195, #1875, #17459, .T. ) ;
#8135 = EDGE_CURVE ( 'NONE', #14793, #13591, #5063, .T. ) ;
#8136 = LINE ( 'NONE', #5161, #3201 ) ;
#8137 = CARTESIAN_POINT ( 'NONE',  ( 0.5889081234606849957, -0.4379237288135600092, 6.978529000034869867 ) ) ;
#8138 = ADVANCED_FACE ( 'NONE', ( #2100 ), #10714, .F. ) ;
#8139 = CARTESIAN_POINT ( 'NONE',  ( -1.981271652668300298, -1.633665147405599871, 5.970160748022450115 ) ) ;
#8140 = DIRECTION ( 'NONE',  ( -1.000000000000000000, -1.168655815394900078E-16, -1.168655815394900078E-16 ) ) ;
#8141 = ADVANCED_FACE ( 'NONE', ( #807 ), #910, .F. ) ;
#8142 = LINE ( 'NONE', #17746, #12718 ) ;
#8143 = CARTESIAN_POINT ( 'NONE',  ( -0.7322514394120432923, -5.586652542372875452, 2.149183891723918993 ) ) ;
#8144 = ORIENTED_EDGE ( 'NONE', *, *, #7245, .T. ) ;
#8145 = SURFACE_STYLE_USAGE ( .BOTH. , #10819 ) ;
#8146 = CARTESIAN_POINT ( 'NONE',  ( -2.500000000000000000, 11.25000000000000000, 7.649999999999999467 ) ) ;
#8147 = CARTESIAN_POINT ( 'NONE',  ( -1.899999999999999911, 9.199999999999999289, 1.600000000000000089 ) ) ;
#8148 = ORIENTED_EDGE ( 'NONE', *, *, #211, .F. ) ;
#8149 = CARTESIAN_POINT ( 'NONE',  ( -0.4790341583531910197, -3.683034516774959855, 2.395814251711740006 ) ) ;
#8150 = CARTESIAN_POINT ( 'NONE',  ( -0.7999999999998790301, 11.40000000000000036, -2.399999999999999911 ) ) ;
#8151 = DIRECTION ( 'NONE',  ( 0.000000000000000000, -1.000000000000000000, 0.000000000000000000 ) ) ;
#8152 = FACE_OUTER_BOUND ( 'NONE', #16676, .T. ) ;
#8153 = CARTESIAN_POINT ( 'NONE',  ( -2.295719155670160383, -3.287133615874060055, 5.218091927917240191 ) ) ;
#8154 = DIRECTION ( 'NONE',  ( 4.318427418585891014E-15, -2.220446049250315053E-16, 1.000000000000000000 ) ) ;
#8155 = CARTESIAN_POINT ( 'NONE',  ( 0.3943683997329633373, -2.215872354612800521, 2.685210827922638543 ) ) ;
#8156 = ADVANCED_FACE ( 'NONE', ( #9222 ), #14885, .F. ) ;
#8157 = LINE ( 'NONE', #1209, #831 ) ;
#8158 = CARTESIAN_POINT ( 'NONE',  ( -1.873832970144350130, -0.2625000000000002331, 2.826167029855650270 ) ) ;
#8159 = ORIENTED_EDGE ( 'NONE', *, *, #2958, .T. ) ;
#8160 = VECTOR ( 'NONE', #11401, 1000.000000000000000 ) ;
#8161 = DIRECTION ( 'NONE',  ( 1.000000000000000000, 0.000000000000000000, 0.000000000000000000 ) ) ;
#8162 = CARTESIAN_POINT ( 'NONE',  ( -0.6864473529425049181, -4.591277760018209975, 6.951118770549909343 ) ) ;
#8163 = VERTEX_POINT ( 'NONE', #4868 ) ;
#8164 = ORIENTED_EDGE ( 'NONE', *, *, #17275, .F. ) ;
#8165 = ORIENTED_EDGE ( 'NONE', *, *, #14460, .F. ) ;
#8166 = CARTESIAN_POINT ( 'NONE',  ( -0.5500000000000000444, 6.450000000000000178, 3.399999999999999911 ) ) ;
#8167 = CARTESIAN_POINT ( 'NONE',  ( 2.051331987628511211, -5.073093220338980025, 4.618035453557344461 ) ) ;
#8168 = EDGE_CURVE ( 'NONE', #12909, #17652, #12115, .T. ) ;
#8169 = ORIENTED_EDGE ( 'NONE', *, *, #13884, .F. ) ;
#8170 = CARTESIAN_POINT ( 'NONE',  ( -0.6150581927481590938, -1.148451969711520082, 6.971662190339330323 ) ) ;
#8171 = DIRECTION ( 'NONE',  ( 2.220446049250309876E-16, -1.000000000000000000, 0.000000000000000000 ) ) ;
#8172 = CARTESIAN_POINT ( 'NONE',  ( -2.316639661709700260, -1.819971453711900056, 4.285359956977770501 ) ) ;
#8173 = CARTESIAN_POINT ( 'NONE',  ( 0.4360591020457930123, -0.008898305084746040497, 2.387347919655840034 ) ) ;
#8174 = ADVANCED_FACE ( 'NONE', ( #7661 ), #12201, .F. ) ;
#8175 = ORIENTED_EDGE ( 'NONE', *, *, #9693, .T. ) ;
#8176 = CARTESIAN_POINT ( 'NONE',  ( -2.143090896833110381, -0.5046610169491529962, 5.672454929438350391 ) ) ;
#8177 = EDGE_LOOP ( 'NONE', ( #8987, #236, #17044, #816 ) ) ;
#8178 = CARTESIAN_POINT ( 'NONE',  ( 1.889104232906359870, -0.04449152542372909747, 3.296507079072520163 ) ) ;
#8179 = EDGE_LOOP ( 'NONE', ( #11449, #1448, #522, #12872 ) ) ;
#8180 = PLANE ( 'NONE',  #7634 ) ;
#8181 = VECTOR ( 'NONE', #16530, 1000.000000000000000 ) ;
#8182 = CARTESIAN_POINT ( 'NONE',  ( 0.2620510901103108581, -1.893677194936739694, 2.361180871966390260 ) ) ;
#8183 = CARTESIAN_POINT ( 'NONE',  ( 2.293398556041700065, -5.364194915254239859, 4.171956209133470317 ) ) ;
#8184 = CARTESIAN_POINT ( 'NONE',  ( -2.652408070456659051, -4.917313796054240349, 4.611427313555255481 ) ) ;
#8185 = ORIENTED_EDGE ( 'NONE', *, *, #13318, .T. ) ;
#8186 = LINE ( 'NONE', #16527, #16419 ) ;
#8187 = CARTESIAN_POINT ( 'NONE',  ( -0.9170541073686521161, -4.315659176918719808, 6.867431071947200039 ) ) ;
#8188 = AXIS2_PLACEMENT_3D ( 'NONE', #11832, #5994, #17454 ) ;
#8189 = CARTESIAN_POINT ( 'NONE',  ( 2.199635523370541357, -0.5429564742160235546, 3.215170965528963531 ) ) ;
#8190 = CARTESIAN_POINT ( 'NONE',  ( -0.5500000000000000444, 0.5999999999999999778, 1.600000000000000089 ) ) ;
#8191 = DIRECTION ( 'NONE',  ( 1.110223024625159992E-16, 0.000000000000000000, -1.000000000000000000 ) ) ;
#8192 = LINE ( 'NONE', #8295, #17119 ) ;
#8193 = CARTESIAN_POINT ( 'NONE',  ( -1.203420131881960398, -1.540511994252448780, 6.363334551077827861 ) ) ;
#8194 = FACE_OUTER_BOUND ( 'NONE', #6493, .T. ) ;
#8195 = VECTOR ( 'NONE', #16996, 1000.000000000000000 ) ;
#8196 = ORIENTED_EDGE ( 'NONE', *, *, #11077, .F. ) ;
#8197 = FACE_OUTER_BOUND ( 'NONE', #352, .T. ) ;
#8198 = CIRCLE ( 'NONE', #17051, 0.6500000000000000222 ) ;
#8199 = CARTESIAN_POINT ( 'NONE',  ( -0.1749999999999999889, 2.700000000000000178, 0.5999999999999999778 ) ) ;
#8200 = VECTOR ( 'NONE', #16439, 1000.000000000000000 ) ;
#8201 = CARTESIAN_POINT ( 'NONE',  ( -1.994315313497099229, -0.2135593220338991571, 5.187224322759965922 ) ) ;
#8202 = CARTESIAN_POINT ( 'NONE',  ( 2.008025181017630167, -2.079983501243050981, 2.964791492240490101 ) ) ;
#8203 = DIRECTION ( 'NONE',  ( -1.908195823574489776E-16, 1.000000000000000000, 1.387778780781449866E-16 ) ) ;
#8204 = MECHANICAL_DESIGN_GEOMETRIC_PRESENTATION_REPRESENTATION (  '', ( #15623 ), #15315 ) ;
#8205 = CARTESIAN_POINT ( 'NONE',  ( -1.864786684738369837, -4.804713230972779137, 2.817120744449669978 ) ) ;
#8206 = CARTESIAN_POINT ( 'NONE',  ( -1.202278654260740876, -5.179872881355935377, 6.364093491318035589 ) ) ;
#8207 = ORIENTED_EDGE ( 'NONE', *, *, #11733, .T. ) ;
#8208 = DIRECTION ( 'NONE',  ( -6.162975822039146519E-33, -0.2588190451025180749, 0.9659258262890690894 ) ) ;
#8209 = LINE ( 'NONE', #2477, #9714 ) ;
#8210 = LINE ( 'NONE', #18087, #14396 ) ;
#8211 = ORIENTED_EDGE ( 'NONE', *, *, #15478, .T. ) ;
#8212 = VECTOR ( 'NONE', #6986, 1000.000000000000000 ) ;
#8213 = CARTESIAN_POINT ( 'NONE',  ( -0.1910247150515231307, -5.595550847457635868, 2.655937705488500722 ) ) ;
#8214 = VECTOR ( 'NONE', #8664, 1000.000000000000000 ) ;
#8215 = CARTESIAN_POINT ( 'NONE',  ( -2.579602008086729459, -4.548542059801595094, 5.323511966907305215 ) ) ;
#8216 = CARTESIAN_POINT ( 'NONE',  ( 2.369027826908510548, -4.009070552811004440, 3.503830760997844518 ) ) ;
#8217 = CARTESIAN_POINT ( 'NONE',  ( -1.000000000000000000, -7.000000000000000000, 5.700000000000000178 ) ) ;
#8218 = CARTESIAN_POINT ( 'NONE',  ( -1.372465729645771182, -1.264893411152960834, 6.226839763556076157 ) ) ;
#8219 = AXIS2_PLACEMENT_3D ( 'NONE', #10830, #16296, #17658 ) ;
#8220 = AXIS2_PLACEMENT_3D ( 'NONE', #14893, #14795, #2108 ) ;
#8221 = CARTESIAN_POINT ( 'NONE',  ( -4.555459529529310125E-17, 5.131370849898479136, 6.100000000000000533 ) ) ;
#8222 = CARTESIAN_POINT ( 'NONE',  ( -1.599999999999880185, 11.40000000000000036, -2.399999999999999911 ) ) ;
#8223 = ORIENTED_EDGE ( 'NONE', *, *, #18172, .T. ) ;
#8224 = AXIS2_PLACEMENT_3D ( 'NONE', #17811, #16354, #2392 ) ;
#8225 = CARTESIAN_POINT ( 'NONE',  ( -1.899999999999999911, 11.15000000000000036, 1.600000000000000089 ) ) ;
#8226 = CARTESIAN_POINT ( 'NONE',  ( 2.645377369053839356, -0.3711864406779670222, 4.488260618344900088 ) ) ;
#8227 = CARTESIAN_POINT ( 'NONE',  ( 1.724579595320000047, -3.939205687946140344, 3.098572228637889836 ) ) ;
#8228 = LINE ( 'NONE', #17923, #9228 ) ;
#8229 = CARTESIAN_POINT ( 'NONE',  ( -0.2000000000000000111, 0.1000000000000000056, 8.300000000000000711 ) ) ;
#8230 = ORIENTED_EDGE ( 'NONE', *, *, #5541, .F. ) ;
#8231 = ORIENTED_EDGE ( 'NONE', *, *, #12648, .F. ) ;
#8232 = CARTESIAN_POINT ( 'NONE',  ( -2.180207327701299658, -5.206567796610168664, 5.586116916730199833 ) ) ;
#8233 = DIRECTION ( 'NONE',  ( 1.000000000000000000, 0.000000000000000000, 0.000000000000000000 ) ) ;
#8234 = CARTESIAN_POINT ( 'NONE',  ( 1.899999999999999911, 2.799999999999999822, 0.5999999999999999778 ) ) ;
#8235 = VECTOR ( 'NONE', #3575, 1000.000000000000000 ) ;
#8236 = VECTOR ( 'NONE', #15464, 1000.000000000000000 ) ;
#8237 = EDGE_CURVE ( 'NONE', #1235, #14775, #3667, .T. ) ;
#8238 = ORIENTED_EDGE ( 'NONE', *, *, #13786, .T. ) ;
#8239 = PRODUCT_RELATED_PRODUCT_CATEGORY ( 'part', '', ( #17748 ) ) ;
#8240 = CARTESIAN_POINT ( 'NONE',  ( -1.282210379528740063, -4.661142624883069630, 6.673494927815290190 ) ) ;
#8241 = EDGE_CURVE ( 'NONE', #1999, #13226, #17539, .T. ) ;
#8242 = AXIS2_PLACEMENT_3D ( 'NONE', #12053, #1867, #7516 ) ;
#8243 =( NAMED_UNIT ( * ) PLANE_ANGLE_UNIT ( ) SI_UNIT ( $, .RADIAN. ) );
#8244 = CARTESIAN_POINT ( 'NONE',  ( -0.5500000000000000444, -2.399999999999999911, 3.600000000000000089 ) ) ;
#8245 = EDGE_CURVE ( 'NONE', #2916, #4730, #16271, .T. ) ;
#8246 = DIRECTION ( 'NONE',  ( -1.110223024625159992E-16, 0.000000000000000000, 1.000000000000000000 ) ) ;
#8247 = EDGE_CURVE ( 'NONE', #3727, #17764, #6260, .T. ) ;
#8248 = CARTESIAN_POINT ( 'NONE',  ( 0.5500000000000000444, 3.050000000000000266, 3.200000000000000178 ) ) ;
#8249 = CARTESIAN_POINT ( 'NONE',  ( -0.8429265834919730249, -2.076142624883080323, 2.502678798553459760 ) ) ;
#8250 = AXIS2_PLACEMENT_3D ( 'NONE', #9795, #11274, #8495 ) ;
#8251 = CYLINDRICAL_SURFACE ( 'NONE', #6993, 0.4000000000000001887 ) ;
#8252 = AXIS2_PLACEMENT_3D ( 'NONE', #8333, #10823, #3881 ) ;
#8253 = CARTESIAN_POINT ( 'NONE',  ( -1.937109463115380903, -3.426863345603793576, 4.019920026366796684 ) ) ;
#8254 = DIRECTION ( 'NONE',  ( -1.048990684667790150E-15, 0.000000000000000000, -1.000000000000000000 ) ) ;
#8255 = CARTESIAN_POINT ( 'NONE',  ( 0.009452110982654818305, -0.3001920447045379747, 2.350000000000000089 ) ) ;
#8256 = EDGE_LOOP ( 'NONE', ( #850, #1082, #14805, #14570 ) ) ;
#8257 = AXIS2_PLACEMENT_3D ( 'NONE', #12900, #12727, #11419 ) ;
#8258 = CARTESIAN_POINT ( 'NONE',  ( -8.881784197001250351E-16, 5.131370849898479136, 6.100000000000000533 ) ) ;
#8259 = CARTESIAN_POINT ( 'NONE',  ( -2.334748642087669523, -4.940602084342530453, 4.403867486184871005 ) ) ;
#8260 = VERTEX_POINT ( 'NONE', #16177 ) ;
#8261 = VERTEX_POINT ( 'NONE', #17818 ) ;
#8262 = PRODUCT_DEFINITION_CONTEXT ( 'detailed design', #1072, 'design' ) ;
#8263 = ORIENTED_EDGE ( 'NONE', *, *, #13790, .T. ) ;
#8264 = LINE ( 'NONE', #18046, #9722 ) ;
#8265 = AXIS2_PLACEMENT_3D ( 'NONE', #17635, #2203, #14989 ) ;
#8266 = CARTESIAN_POINT ( 'NONE',  ( -2.012177589105470066, -5.215466101694915757, 5.107213040360599088 ) ) ;
#8267 = CARTESIAN_POINT ( 'NONE',  ( -0.2010642693394331104, -1.847100618360169699, 2.053740970238008501 ) ) ;
#8268 = ADVANCED_FACE ( 'NONE', ( #14985 ), #7949, .T. ) ;
#8269 = CARTESIAN_POINT ( 'NONE',  ( -2.500000000000000000, 9.199999999999999289, 1.600000000000000089 ) ) ;
#8270 = DIRECTION ( 'NONE',  ( -6.083413833562510128E-16, 1.520853458390629997E-16, -1.000000000000000000 ) ) ;
#8271 = CARTESIAN_POINT ( 'NONE',  ( -1.255262969126040791E-16, 2.049999999999999822, 5.100000000000000533 ) ) ;
#8272 = CARTESIAN_POINT ( 'NONE',  ( -1.899999999999999911, 0.5999999999999999778, 7.550000000000000711 ) ) ;
#8273 = CARTESIAN_POINT ( 'NONE',  ( 1.899999999999999911, 11.29999999999999893, 1.600000000000000089 ) ) ;
#8274 = CARTESIAN_POINT ( 'NONE',  ( 0.1749999999999999889, 9.299999999999998934, 1.600000000000000089 ) ) ;
#8275 = CARTESIAN_POINT ( 'NONE',  ( -1.710920205120030069, -1.587088570829020107, 6.316012914303580139 ) ) ;
#8276 = CARTESIAN_POINT ( 'NONE',  ( -2.043014502273419186, -0.2580508474576271305, 3.006203457898251052 ) ) ;
#8277 = CARTESIAN_POINT ( 'NONE',  ( 0.3743405594629510280, -0.4423728813559330009, 7.023440622744399953 ) ) ;
#8278 = AXIS2_PLACEMENT_3D ( 'NONE', #209, #15589, #11233 ) ;
#8279 = ORIENTED_EDGE ( 'NONE', *, *, #15234, .F. ) ;
#8280 = CARTESIAN_POINT ( 'NONE',  ( -1.300961508564169922, -0.1779661016949160013, 6.661123742937279602 ) ) ;
#8281 = CARTESIAN_POINT ( 'NONE',  ( 1.652654650382400003, -0.7952867690272209522, 3.029252778805629820 ) ) ;
#8282 = VERTEX_POINT ( 'NONE', #4968 ) ;
#8283 = LINE ( 'NONE', #14008, #260 ) ;
#8284 = CARTESIAN_POINT ( 'NONE',  ( 2.326448859701049976, -2.219713230972779616, 4.344498395672271585 ) ) ;
#8285 = CARTESIAN_POINT ( 'NONE',  ( 2.578017356471871135, -5.386440677966105817, 5.329826563567761077 ) ) ;
#8286 = EDGE_CURVE ( 'NONE', #1735, #11364, #3762, .T. ) ;
#8287 = EDGE_LOOP ( 'NONE', ( #12217, #8263, #9803, #8564 ) ) ;
#8288 = CARTESIAN_POINT ( 'NONE',  ( 2.351212046067109984, -0.9815930753335269099, 4.597298481426010497 ) ) ;
#8289 = CARTESIAN_POINT ( 'NONE',  ( 1.000000000000000000, -5.599999999999999645, 3.673738709727309981 ) ) ;
#8290 = VECTOR ( 'NONE', #12571, 1000.000000000000000 ) ;
#8291 = CARTESIAN_POINT ( 'NONE',  ( -1.803891155489810050, -4.781424942684489920, 3.188470185434129966 ) ) ;
#8292 = ORIENTED_EDGE ( 'NONE', *, *, #3141, .T. ) ;
#8293 = LINE ( 'NONE', #13932, #11712 ) ;
#8294 = CARTESIAN_POINT ( 'NONE',  ( 1.750000000000060174, 0.5999999999999999778, 7.550000000000000711 ) ) ;
#8295 = CARTESIAN_POINT ( 'NONE',  ( 1.399999999999999911, -5.500000000000000000, 5.100000000000000533 ) ) ;
#8296 = CARTESIAN_POINT ( 'NONE',  ( -1.688800633088611836, -4.758136654396205145, 3.532586505616431616 ) ) ;
#8297 = EDGE_CURVE ( 'NONE', #14464, #17808, #7843, .T. ) ;
#8298 = LINE ( 'NONE', #5335, #5248 ) ;
#8299 = ORIENTED_EDGE ( 'NONE', *, *, #4595, .F. ) ;
#8300 = CARTESIAN_POINT ( 'NONE',  ( -4.898587196589392737E-17, 6.700000000000000178, 6.349999999999999645 ) ) ;
#8301 = DIRECTION ( 'NONE',  ( 1.224646799147350002E-16, -1.000000000000000000, -6.123233995736769734E-17 ) ) ;
#8302 = CARTESIAN_POINT ( 'NONE',  ( -0.2453710345350140487, -0.1557203389830511819, 6.738252723719333481 ) ) ;
#8303 = CARTESIAN_POINT ( 'NONE',  ( -2.174104834890490778, -4.455388906648449776, 6.221966445066275497 ) ) ;
#8304 = ORIENTED_EDGE ( 'NONE', *, *, #711, .T. ) ;
#8305 = AXIS2_PLACEMENT_3D ( 'NONE', #3748, #5240, #12100 ) ;
#8306 = CARTESIAN_POINT ( 'NONE',  ( -1.385366411767399608, -5.164643153926310681, 2.415423146782709640 ) ) ;
#8307 = CARTESIAN_POINT ( 'NONE',  ( -0.3803919826357066158, -5.291101694915254505, 2.682580100125310896 ) ) ;
#8308 = VERTEX_POINT ( 'NONE', #6233 ) ;
#8309 = FACE_OUTER_BOUND ( 'NONE', #9892, .T. ) ;
#8310 = PLANE ( 'NONE',  #11179 ) ;
#8311 = CARTESIAN_POINT ( 'NONE',  ( -1.661700935788390066, -0.5625000000000000000, 3.038299064211610112 ) ) ;
#8312 = EDGE_CURVE ( 'NONE', #6036, #8906, #14393, .T. ) ;
#8313 = CARTESIAN_POINT ( 'NONE',  ( -0.8570167067220350043, -5.582203389830509899, 2.508190348879359988 ) ) ;
#8314 = CARTESIAN_POINT ( 'NONE',  ( 2.556942001999820580, -3.756740257999804378, 3.989253004641562406 ) ) ;
#8315 = CARTESIAN_POINT ( 'NONE',  ( -2.649291707874080970, -3.356998480738929924, 4.543900225523854530 ) ) ;
#8316 = DIRECTION ( 'NONE',  ( 1.000000000000000000, 0.000000000000000000, 1.850371707708589879E-16 ) ) ;
#8317 = AXIS2_PLACEMENT_3D ( 'NONE', #11263, #7192, #11070 ) ;
#8318 = CARTESIAN_POINT ( 'NONE',  ( -2.044452488559148851, -1.451199717459271454, 4.887392274793804781 ) ) ;
#8319 = DIRECTION ( 'NONE',  ( -1.000000000000000000, 1.073215590470990073E-14, -1.110223024625159992E-16 ) ) ;
#8320 = ORIENTED_EDGE ( 'NONE', *, *, #8581, .T. ) ;
#8321 = CARTESIAN_POINT ( 'NONE',  ( 1.752210068153130074, -5.105895474282090341, 2.947789931846859890 ) ) ;
#8322 = SHAPE_REPRESENTATION ( 'Switch Metal Shield Frame', ( #17681 ), #12094 ) ;
#8323 = CARTESIAN_POINT ( 'NONE',  ( -2.234315482767910144, -0.5402542372881360411, 3.960850823455329905 ) ) ;
#8324 = CARTESIAN_POINT ( 'NONE',  ( 0.1226612266411070129, -2.937809291549740021, 7.050255286338659388 ) ) ;
#8325 = DIRECTION ( 'NONE',  ( 0.000000000000000000, -1.000000000000000000, 0.000000000000000000 ) ) ;
#8326 = CARTESIAN_POINT ( 'NONE',  ( 2.321479326063749404, -5.050847457627124726, 3.414080590619961608 ) ) ;
#8327 = ORIENTED_EDGE ( 'NONE', *, *, #11796, .T. ) ;
#8328 = PRODUCT_DEFINITION_SHAPE ( 'NONE', 'NONE',  #17933 ) ;
#8329 = LINE ( 'NONE', #6564, #14923 ) ;
#8330 = ORIENTED_EDGE ( 'NONE', *, *, #1555, .T. ) ;
#8331 = EDGE_CURVE ( 'NONE', #10942, #14423, #9403, .T. ) ;
#8332 = CARTESIAN_POINT ( 'NONE',  ( -1.699999999999999956, 2.299999999999999822, 7.599999999999999645 ) ) ;
#8333 = CARTESIAN_POINT ( 'NONE',  ( -1.000000000000000000, 5.799999999999999822, 7.700000000000000178 ) ) ;
#8334 = EDGE_LOOP ( 'NONE', ( #17219, #2234, #17813, #1689, #5079, #5962, #12297, #6976, #3750, #9786, #8320, #10748, #13859, #7805, #1949, #923, #10648, #15516, #6211, #2163, #15395, #8526, #10293, #15297 ) ) ;
#8335 = CARTESIAN_POINT ( 'NONE',  ( -0.8986180677147959095, -3.636457940198390304, 2.524860635301629852 ) ) ;
#8336 = CARTESIAN_POINT ( 'NONE',  ( 0.1749999999999999889, 9.299999999999998934, 1.600000000000000089 ) ) ;
#8337 = CARTESIAN_POINT ( 'NONE',  ( 1.104321075428930765, -5.320452325212860600, 2.282937282173381099 ) ) ;
#8338 = DIRECTION ( 'NONE',  ( 0.000000000000000000, 0.7492686492653550800, -0.6622661785325221206 ) ) ;
#8339 = PLANE ( 'NONE',  #5542 ) ;
#8340 = CARTESIAN_POINT ( 'NONE',  ( -0.03714311608457869507, -4.521412895153340550, 7.053160869216429596 ) ) ;
#8341 = CARTESIAN_POINT ( 'NONE',  ( 1.899999999999999911, 0.5999999999999999778, 7.550000000000000711 ) ) ;
#8342 = CARTESIAN_POINT ( 'NONE',  ( -1.951270856817509003, -3.263845327585779277, 5.338313313320930398 ) ) ;
#8343 = PLANE ( 'NONE',  #17368 ) ;
#8344 = VERTEX_POINT ( 'NONE', #17333 ) ;
#8345 = LINE ( 'NONE', #1299, #10946 ) ;
#8346 = ORIENTED_EDGE ( 'NONE', *, *, #782, .T. ) ;
#8347 = EDGE_CURVE ( 'NONE', #16569, #17897, #7458, .T. ) ;
#8348 = MANIFOLD_SOLID_BREP ( 'Stock-MAS-687-1', #14386 ) ;
#8349 = CARTESIAN_POINT ( 'NONE',  ( -2.281778813005780115, -4.847448931189379806, 5.276394947932169899 ) ) ;
#8350 = VERTEX_POINT ( 'NONE', #13178 ) ;
#8351 = ADVANCED_FACE ( 'NONE', ( #1629 ), #1967, .T. ) ;
#8352 = ORIENTED_EDGE ( 'NONE', *, *, #8922, .T. ) ;
#8353 = ORIENTED_EDGE ( 'NONE', *, *, #16840, .T. ) ;
#8354 = FACE_OUTER_BOUND ( 'NONE', #5218, .T. ) ;
#8355 = CARTESIAN_POINT ( 'NONE',  ( -0.6964468257805866980, -5.166525423728809407, 6.631228347243847132 ) ) ;
#8356 = DIRECTION ( 'NONE',  ( 6.083413833562498788E-17, 3.041706916781249394E-17, 1.000000000000000000 ) ) ;
#8357 = DIRECTION ( 'NONE',  ( -1.000000000000000000, 0.000000000000000000, 0.000000000000000000 ) ) ;
#8358 = CARTESIAN_POINT ( 'NONE',  ( 1.899999999999999911, 10.00000000000000000, 0.5999999999999999778 ) ) ;
#8359 = CARTESIAN_POINT ( 'NONE',  ( -1.899999999999999911, 10.00000000000000000, 5.075305255429290705E-16 ) ) ;
#8360 = DIRECTION ( 'NONE',  ( 0.000000000000000000, -1.000000000000000000, 0.000000000000000000 ) ) ;
#8361 = CARTESIAN_POINT ( 'NONE',  ( 0.9170541073686970801, -1.284340823081270067, 6.867431071947180499 ) ) ;
#8362 = CARTESIAN_POINT ( 'NONE',  ( 0.6470883152343921418, -2.569037555297099651, 6.648378442427241630 ) ) ;
#8363 = CARTESIAN_POINT ( 'NONE',  ( -1.791574935211209807, -0.1913135593220340047, 6.226029630577610163 ) ) ;
#8364 = EDGE_CURVE ( 'NONE', #3530, #1479, #16139, .T. ) ;
#8365 = AXIS2_PLACEMENT_3D ( 'NONE', #18016, #5363, #18101 ) ;
#8366 = CARTESIAN_POINT ( 'NONE',  ( 1.000896394980339998, -0.4290254237288140260, 6.829956240957369751 ) ) ;
#8367 = CARTESIAN_POINT ( 'NONE',  ( -1.994315313497099229, -0.5135593220338985354, 5.187224322759965922 ) ) ;
#8368 = DIRECTION ( 'NONE',  ( -4.177994306516050823E-17, 0.7310552682428690385, -0.6823182503600111470 ) ) ;
#8369 = ORIENTED_EDGE ( 'NONE', *, *, #6390, .T. ) ;
#8370 = EDGE_CURVE ( 'NONE', #15079, #8647, #12917, .T. ) ;
#8371 = CARTESIAN_POINT ( 'NONE',  ( -0.4974685680287780354, -0.1601694915254240070, 7.000224381598740386 ) ) ;
#8372 = CARTESIAN_POINT ( 'NONE',  ( 2.145694642186089851, -1.098034516774969882, 5.666819626392539888 ) ) ;
#8373 = ORIENTED_EDGE ( 'NONE', *, *, #15264, .T. ) ;
#8374 = EDGE_CURVE ( 'NONE', #14568, #13591, #4479, .T. ) ;
#8375 = PLANE ( 'NONE',  #12682 ) ;
#8376 = VERTEX_POINT ( 'NONE', #10683 ) ;
#8377 = CARTESIAN_POINT ( 'NONE',  ( -1.397172971746989178, -1.707370888630439731, 2.806153814454940054 ) ) ;
#8378 = CARTESIAN_POINT ( 'NONE',  ( 0.7998959936908462964, -5.435381355932195291, 7.230419212249866945 ) ) ;
#8379 = ORIENTED_EDGE ( 'NONE', *, *, #3843, .F. ) ;
#8380 = CARTESIAN_POINT ( 'NONE',  ( 1.901882987994760965, -0.3934322033898309257, 5.472995608211450147 ) ) ;
#8381 = ORIENTED_EDGE ( 'NONE', *, *, #13906, .F. ) ;
#8382 = DIRECTION ( 'NONE',  ( -7.340317518182859527E-17, 0.000000000000000000, -1.000000000000000000 ) ) ;
#8383 = DIRECTION ( 'NONE',  ( 0.000000000000000000, 0.000000000000000000, 1.000000000000000000 ) ) ;
#8384 = DIRECTION ( 'NONE',  ( -0.000000000000000000, 1.000000000000000000, 0.000000000000000000 ) ) ;
#8385 = CARTESIAN_POINT ( 'NONE',  ( 0.05638445020230590382, -1.377493976234431372, 6.752248190741917178 ) ) ;
#8386 = CARTESIAN_POINT ( 'NONE',  ( -0.03000000000000110217, 11.40000000000000036, 7.649999999999999467 ) ) ;
#8387 = ORIENTED_EDGE ( 'NONE', *, *, #11852, .T. ) ;
#8388 = CARTESIAN_POINT ( 'NONE',  ( 1.500000000000000000, -5.599999999999999645, 2.299999999999999822 ) ) ;
#8389 = DIRECTION ( 'NONE',  ( -1.101047627727429853E-16, 0.000000000000000000, 1.000000000000000000 ) ) ;
#8390 = CARTESIAN_POINT ( 'NONE',  ( 0.06367493584606445656, -0.3014830508474583004, 2.649999999999998579 ) ) ;
#8391 = EDGE_CURVE ( 'NONE', #17750, #10646, #675, .T. ) ;
#8392 = CARTESIAN_POINT ( 'NONE',  ( 1.752195476665078688, -4.036199717459260761, 6.693219682964302031 ) ) ;
#8393 = LINE ( 'NONE', #14029, #13512 ) ;
#8394 = CARTESIAN_POINT ( 'NONE',  ( 0.7982439214406963357, -5.130932203389829915, 6.591424794228156081 ) ) ;
#8395 = EDGE_LOOP ( 'NONE', ( #5595, #287, #1909, #15814 ) ) ;
#8396 = CARTESIAN_POINT ( 'NONE',  ( 1.378221871957439504, -0.1201271186440679983, 6.607619368096267820 ) ) ;
#8397 = CARTESIAN_POINT ( 'NONE',  ( -2.500000000000000000, 2.799999999999999822, 1.600000000000000089 ) ) ;
#8398 = DIRECTION ( 'NONE',  ( -1.224646799147341128E-16, -1.000000000000000000, 0.000000000000000000 ) ) ;
#8399 = ORIENTED_EDGE ( 'NONE', *, *, #10613, .T. ) ;
#8400 = DIRECTION ( 'NONE',  ( 0.000000000000000000, 0.000000000000000000, -1.000000000000000000 ) ) ;
#8401 = CARTESIAN_POINT ( 'NONE',  ( -1.567709126316399804, -1.684082600342149849, 2.944712621036610134 ) ) ;
#8402 = ADVANCED_FACE ( 'NONE', ( #9477 ), #17875, .T. ) ;
#8403 = CARTESIAN_POINT ( 'NONE',  ( -0.4000000000000000222, 2.399999999999999911, 5.100000000000000533 ) ) ;
#8404 =( REPRESENTATION_RELATIONSHIP ('NONE','NONE', #2757, #853 ) REPRESENTATION_RELATIONSHIP_WITH_TRANSFORMATION ( #10758 )SHAPE_REPRESENTATION_RELATIONSHIP( ) );
#8405 = LINE ( 'NONE', #12664, #18221 ) ;
#8406 = ORIENTED_EDGE ( 'NONE', *, *, #12820, .F. ) ;
#8407 = EDGE_CURVE ( 'NONE', #16536, #1995, #10580, .T. ) ;
#8408 = LINE ( 'NONE', #7019, #12384 ) ;
#8409 = CARTESIAN_POINT ( 'NONE',  ( 0.3743405594629510280, -0.4423728813559330009, 7.023440622744399953 ) ) ;
#8410 = CARTESIAN_POINT ( 'NONE',  ( 2.337178851518220135, -2.588484967225419986, 4.976298214796759822 ) ) ;
#8411 = DIRECTION ( 'NONE',  ( 0.000000000000000000, -1.000000000000000000, -2.220446049250309876E-16 ) ) ;
#8412 = LINE ( 'NONE', #9983, #6 ) ;
#8413 = CARTESIAN_POINT ( 'NONE',  ( 2.508228811380011081, -5.090889830508485758, 5.566973598334535644 ) ) ;
#8414 = ORIENTED_EDGE ( 'NONE', *, *, #9286, .T. ) ;
#8415 = VERTEX_POINT ( 'NONE', #16235 ) ;
#8416 = CARTESIAN_POINT ( 'NONE',  ( -0.4058874503045720172, 7.799999999999999822, 6.100000000000000533 ) ) ;
#8417 = CARTESIAN_POINT ( 'NONE',  ( 1.889999999999999902, 8.500000000000000000, 0.6099999999999999867 ) ) ;
#8418 = DIRECTION ( 'NONE',  ( -2.986159789035700404E-15, 1.110223024625159992E-16, 1.000000000000000000 ) ) ;
#8419 = VERTEX_POINT ( 'NONE', #3540 ) ;
#8420 = CARTESIAN_POINT ( 'NONE',  ( -0.009452110982655139229, -5.299807955295460005, 2.350000000000000089 ) ) ;
#8421 = DIRECTION ( 'NONE',  ( 0.000000000000000000, -1.000000000000000000, 0.000000000000000000 ) ) ;
#8422 = CARTESIAN_POINT ( 'NONE',  ( -2.500000000000000000, 2.799999999999999822, 1.600000000000000089 ) ) ;
#8423 =( BOUNDED_CURVE ( )  B_SPLINE_CURVE ( 3, ( #15700, #4111, #15432, #4387 ),
 .UNSPECIFIED., .F., .F. ) 
 B_SPLINE_CURVE_WITH_KNOTS ( ( 4, 4 ),
 ( 0.000000000000000000, 1.000000000000000000 ),
 .UNSPECIFIED. ) 
 CURVE ( )  GEOMETRIC_REPRESENTATION_ITEM ( )  RATIONAL_B_SPLINE_CURVE ( ( 1.000000000000000000, 0.8047378541243649375, 0.8047378541243649375, 1.000000000000000000 ) ) 
 REPRESENTATION_ITEM ( '' )  );
#8424 = CARTESIAN_POINT ( 'NONE',  ( 2.102728310581320148, -4.241953435693879726, 5.757014351541050345 ) ) ;
#8425 = CARTESIAN_POINT ( 'NONE',  ( 1.000000000000000000, 6.400000000000000355, 7.700000000000000178 ) ) ;
#8426 = CARTESIAN_POINT ( 'NONE',  ( -1.583713126240711588, -3.170692174432623744, 6.006428174987420654 ) ) ;
#8427 = CARTESIAN_POINT ( 'NONE',  ( 1.899999999999999911, 9.199999999999999289, 1.600000000000000089 ) ) ;
#8428 = CARTESIAN_POINT ( 'NONE',  ( 1.399999999999999911, -8.000000000000000000, 3.299999999999999822 ) ) ;
#8429 = ORIENTED_EDGE ( 'NONE', *, *, #1449, .T. ) ;
#8430 = FACE_OUTER_BOUND ( 'NONE', #1050, .T. ) ;
#8431 = ORIENTED_EDGE ( 'NONE', *, *, #10600, .F. ) ;
#8432 = DIRECTION ( 'NONE',  ( 3.018987445473099952E-48, 1.000000000000000000, 2.465190328815659976E-32 ) ) ;
#8433 = VERTEX_POINT ( 'NONE', #11394 ) ;
#8434 = VERTEX_POINT ( 'NONE', #17117 ) ;
#8435 = DIRECTION ( 'NONE',  ( 0.000000000000000000, -1.000000000000000000, 0.000000000000000000 ) ) ;
#8436 = PRODUCT_DEFINITION_CONTEXT ( 'detailed design', #4946, 'design' ) ;
#8437 = VERTEX_POINT ( 'NONE', #15838 ) ;
#8438 = CARTESIAN_POINT ( 'NONE',  ( -0.07299321914061848715, -5.298516949152539901, 2.350000000000000089 ) ) ;
#8439 = CARTESIAN_POINT ( 'NONE',  ( 1.011820239713300484, -1.963542059801608897, 2.246566997958089118 ) ) ;
#8440 = DIRECTION ( 'NONE',  ( 6.083413833562510128E-16, -1.647588903766454767E-16, 1.000000000000000000 ) ) ;
#8441 = CARTESIAN_POINT ( 'NONE',  ( 1.732393070546229819, -0.7511144650864829408, 2.954861780286969886 ) ) ;
#8442 = LINE ( 'NONE', #1404, #14090 ) ;
#8443 = LINE ( 'NONE', #14190, #5494 ) ;
#8444 = PLANE ( 'NONE',  #11181 ) ;
#8445 = EDGE_CURVE ( 'NONE', #16779, #616, #17282, .T. ) ;
#8446 = CARTESIAN_POINT ( 'NONE',  ( 2.211317922628870392, -2.472043525783979678, 3.894507149290419967 ) ) ;
#8447 = CARTESIAN_POINT ( 'NONE',  ( 0.5549238885286489342, -3.500569086828633658, 2.723396519134821059 ) ) ;
#8448 = CARTESIAN_POINT ( 'NONE',  ( 0.1565249325564390115, -0.1468220338983060036, 7.048192310558509810 ) ) ;
#8449 = DIRECTION ( 'NONE',  ( 0.000000000000000000, -1.000000000000000000, 0.000000000000000000 ) ) ;
#8450 = CARTESIAN_POINT ( 'NONE',  ( 1.000000000000000000, 5.799999999999999822, 8.300000000000000711 ) ) ;
#8451 = ORIENTED_EDGE ( 'NONE', *, *, #2935, .F. ) ;
#8452 = CARTESIAN_POINT ( 'NONE',  ( -2.293398556041709835, -0.2358050847457629773, 4.171956209133480975 ) ) ;
#8453 = CARTESIAN_POINT ( 'NONE',  ( 2.126557263589630153, -2.448755237495689574, 3.691783806836010040 ) ) ;
#8454 = VERTEX_POINT ( 'NONE', #13054 ) ;
#8455 = ADVANCED_FACE ( 'NONE', ( #4254 ), #373, .F. ) ;
#8456 = VERTEX_POINT ( 'NONE', #17026 ) ;
#8457 = CARTESIAN_POINT ( 'NONE',  ( 0.6918414964981907112, -1.940253771513320125, 2.450533167346752084 ) ) ;
#8458 = DIRECTION ( 'NONE',  ( 1.000000000000000000, 0.000000000000000000, 0.000000000000000000 ) ) ;
#8459 = CARTESIAN_POINT ( 'NONE',  ( -1.596341326794979976, -5.564406779661021041, 2.970780074643819990 ) ) ;
#8460 = ORIENTED_EDGE ( 'NONE', *, *, #6216, .F. ) ;
#8461 = EDGE_CURVE ( 'NONE', #1300, #9201, #10012, .T. ) ;
#8462 = CARTESIAN_POINT ( 'NONE',  ( 0.4985810152601650724, -1.330917399657850053, 7.000035360316460675 ) ) ;
#8463 = AXIS2_PLACEMENT_3D ( 'NONE', #10538, #3603, #9252 ) ;
#8464 = CARTESIAN_POINT ( 'NONE',  ( -2.000624272291700034, -0.5358050847457624943, 4.239366054776020576 ) ) ;
#8465 = EDGE_LOOP ( 'NONE', ( #3080, #8369, #3321, #10212 ) ) ;
#8466 = ADVANCED_FACE ( 'NONE', ( #3060 ), #7412, .T. ) ;
#8467 = CARTESIAN_POINT ( 'NONE',  ( 0.5000000000000000000, 3.500000000000000000, 5.100000000000000533 ) ) ;
#8468 = LINE ( 'NONE', #2824, #17651 ) ;
#8469 = DIRECTION ( 'NONE',  ( -2.220446049250309876E-16, -1.000000000000000000, 4.958742624062499518E-17 ) ) ;
#8470 = EDGE_CURVE ( 'NONE', #16824, #12466, #7231, .T. ) ;
#8471 = CARTESIAN_POINT ( 'NONE',  ( 1.259207372045950457, -2.332313796054251487, 3.078488779929903441 ) ) ;
#8472 = EDGE_CURVE ( 'NONE', #14839, #2212, #7352, .T. ) ;
#8473 = CARTESIAN_POINT ( 'NONE',  ( -1.899999999999999911, 11.15000000000000036, 7.990820364436479856E-16 ) ) ;
#8474 = ORIENTED_EDGE ( 'NONE', *, *, #5878, .F. ) ;
#8475 = DIRECTION ( 'NONE',  ( -0.6614378277661479011, 8.100277186087908528E-17, -0.7499999999999997780 ) ) ;
#8476 = PLANE ( 'NONE',  #6434 ) ;
#8477 = AXIS2_PLACEMENT_3D ( 'NONE', #10202, #8833, #15781 ) ;
#8478 = DIRECTION ( 'NONE',  ( 1.000000000000000000, -1.445602896647339114E-15, 2.891205793294678228E-15 ) ) ;
#8479 = CARTESIAN_POINT ( 'NONE',  ( 0.2453710345350221533, -5.444279661016954819, 6.738252723719333481 ) ) ;
#8480 = ORIENTED_EDGE ( 'NONE', *, *, #10102, .F. ) ;
#8481 = DIRECTION ( 'NONE',  ( -1.000000000000000000, 0.000000000000000000, 0.000000000000000000 ) ) ;
#8482 = DIRECTION ( 'NONE',  ( 1.000000000000000000, -2.960594732333750117E-16, 0.000000000000000000 ) ) ;
#8483 = PLANE ( 'NONE',  #1969 ) ;
#8484 = ORIENTED_EDGE ( 'NONE', *, *, #17947, .T. ) ;
#8485 = FACE_OUTER_BOUND ( 'NONE', #13050, .T. ) ;
#8486 = CIRCLE ( 'NONE', #13247, 0.09999999999999997780 ) ;
#8487 = CARTESIAN_POINT ( 'NONE',  ( 0.6864473529425539899, -1.008722239981789892, 6.951118770549889803 ) ) ;
#8488 = ADVANCED_FACE ( 'NONE', ( #10101 ), #15753, .T. ) ;
#8489 = VECTOR ( 'NONE', #6001, 1000.000000000000000 ) ;
#8490 = DIRECTION ( 'NONE',  ( 0.7071067811865489050, 0.000000000000000000, -0.7071067811865461294 ) ) ;
#8491 = CARTESIAN_POINT ( 'NONE',  ( -1.909909196654771213, -1.567641158900710430, 3.946907241329710381 ) ) ;
#8492 = LINE ( 'NONE', #7199, #1100 ) ;
#8493 = VERTEX_POINT ( 'NONE', #15572 ) ;
#8494 = AXIS2_PLACEMENT_3D ( 'NONE', #11727, #10341, #14514 ) ;
#8495 = DIRECTION ( 'NONE',  ( -0.3420201433256691015, 0.000000000000000000, 0.9396926207859082059 ) ) ;
#8496 = CARTESIAN_POINT ( 'NONE',  ( -2.058670345754650022, -0.5491525423728820243, 3.559656372813929881 ) ) ;
#8497 = CARTESIAN_POINT ( 'NONE',  ( -2.219956784870669608, -3.426863345603790023, 3.918630970161619764 ) ) ;
#8498 = FACE_OUTER_BOUND ( 'NONE', #1965, .T. ) ;
#8499 = CARTESIAN_POINT ( 'NONE',  ( 4.225031457058369810E-16, 2.299999999999999822, 7.599999999999999645 ) ) ;
#8500 = CARTESIAN_POINT ( 'NONE',  ( 0.07064654565475687875, -5.448728813559320372, 7.352897294663512717 ) ) ;
#8501 = VERTEX_POINT ( 'NONE', #14445 ) ;
#8502 = VECTOR ( 'NONE', #8756, 1000.000000000000000 ) ;
#8503 = VECTOR ( 'NONE', #5818, 1000.000000000000000 ) ;
#8504 = VERTEX_POINT ( 'NONE', #6013 ) ;
#8505 = DIRECTION ( 'NONE',  ( -1.000000000000000000, 1.480297366166879989E-15, 0.000000000000000000 ) ) ;
#8506 = CARTESIAN_POINT ( 'NONE',  ( -2.500000000000000000, 10.00000000000000000, 7.654042494670959579E-16 ) ) ;
#8507 = EDGE_LOOP ( 'NONE', ( #14502, #4685, #11623, #14880 ) ) ;
#8508 = AXIS2_PLACEMENT_3D ( 'NONE', #1680, #7329, #9837 ) ;
#8509 = CIRCLE ( 'NONE', #17070, 0.4000000000000000222 ) ;
#8510 = CARTESIAN_POINT ( 'NONE',  ( -1.558664967382870525, -1.540511994252448780, 6.847947208954447973 ) ) ;
#8511 = VECTOR ( 'NONE', #7337, 1000.000000000000000 ) ;
#8512 = EDGE_CURVE ( 'NONE', #2252, #2042, #12873, .T. ) ;
#8513 = CARTESIAN_POINT ( 'NONE',  ( -0.009452110982655142699, -0.5998079552954631577, 2.050000000000001155 ) ) ;
#8514 = CARTESIAN_POINT ( 'NONE',  ( 0.6536199613480476733, -5.011796459788070202, 2.109674034588110647 ) ) ;
#8515 = DIRECTION ( 'NONE',  ( -1.000000000000000000, -1.746418240983389920E-16, -1.110223024625159992E-16 ) ) ;
#8516 = CARTESIAN_POINT ( 'NONE',  ( -0.8242394280876599311, -1.171740257999809964, 6.904399023015030501 ) ) ;
#8517 = LINE ( 'NONE', #14167, #14998 ) ;
#8518 = AXIS2_PLACEMENT_3D ( 'NONE', #16445, #3382, #7743 ) ;
#8519 = CARTESIAN_POINT ( 'NONE',  ( 1.994983296312400123, -4.265241723982169830, 5.948514050749290405 ) ) ;
#8520 = PLANE ( 'NONE',  #15568 ) ;
#8521 = CARTESIAN_POINT ( 'NONE',  ( 0.6713553523423281266, -2.867944426684881254, 6.640150466718861999 ) ) ;
#8522 = FACE_OUTER_BOUND ( 'NONE', #7937, .T. ) ;
#8523 = FACE_OUTER_BOUND ( 'NONE', #2979, .T. ) ;
#8525 = VECTOR ( 'NONE', #8107, 1000.000000000000000 ) ;
#8524 = AXIS2_PLACEMENT_3D ( 'NONE', #5154, #9032, #6549 ) ;
#8526 = ORIENTED_EDGE ( 'NONE', *, *, #211, .T. ) ;
#8527 = CARTESIAN_POINT ( 'NONE',  ( -1.899999999999999911, 11.25000000000000000, 7.649999999999999467 ) ) ;
#8528 = VERTEX_POINT ( 'NONE', #2791 ) ;
#8529 = CIRCLE ( 'NONE', #10283, 0.6100000000000000977 ) ;
#8530 = CARTESIAN_POINT ( 'NONE',  ( 1.000000000000000000, 5.799999999999999822, 7.700000000000000178 ) ) ;
#8531 = VERTEX_POINT ( 'NONE', #14071 ) ;
#8532 = DIRECTION ( 'NONE',  ( 2.220446049250309876E-16, 0.000000000000000000, -1.000000000000000000 ) ) ;
#8533 = VECTOR ( 'NONE', #13912, 1000.000000000000000 ) ;
#8534 = VECTOR ( 'NONE', #5519, 1000.000000000000000 ) ;
#8535 = ORIENTED_EDGE ( 'NONE', *, *, #11874, .T. ) ;
#8536 = CARTESIAN_POINT ( 'NONE',  ( 1.880631435828169939, -5.055296610169490279, 3.876649216148224220 ) ) ;
#8537 = DIRECTION ( 'NONE',  ( 1.224646799147350002E-16, -1.000000000000000000, -6.123233995736779594E-17 ) ) ;
#8538 = CARTESIAN_POINT ( 'NONE',  ( 1.757131520353529819, -0.5645261550885040114, 2.952711384047340015 ) ) ;
#8539 = VECTOR ( 'NONE', #5632, 1000.000000000000000 ) ;
#8540 = CARTESIAN_POINT ( 'NONE',  ( 0.7500000000000000000, 3.050000000000000266, 2.699264068711930253 ) ) ;
#8541 = CIRCLE ( 'NONE', #1732, 0.01000000000000002623 ) ;
#8542 = LINE ( 'NONE', #8359, #11993 ) ;
#8543 = VECTOR ( 'NONE', #10855, 1000.000000000000000 ) ;
#8544 = DIRECTION ( 'NONE',  ( 2.986159789035700404E-15, -1.110223024625159992E-16, -1.000000000000000000 ) ) ;
#8545 = LINE ( 'NONE', #1509, #15358 ) ;
#8546 = CARTESIAN_POINT ( 'NONE',  ( -2.219956784870669608, -3.426863345603790023, 3.918630970161619764 ) ) ;
#8547 = CARTESIAN_POINT ( 'NONE',  ( 1.520647680314149541, -3.640298816558361406, 3.320676805464615633 ) ) ;
#8548 = CARTESIAN_POINT ( 'NONE',  ( 2.052786957354850728, -0.07563559322033948373, 4.727327971967373976 ) ) ;
#8549 = DIRECTION ( 'NONE',  ( 0.000000000000000000, -1.000000000000000000, 0.000000000000000000 ) ) ;
#8550 = DIRECTION ( 'NONE',  ( 0.000000000000000000, 1.000000000000000000, 0.000000000000000000 ) ) ;
#8551 = ORIENTED_EDGE ( 'NONE', *, *, #6092, .F. ) ;
#8552 = CARTESIAN_POINT ( 'NONE',  ( 2.253200202764420013, -0.08898305084745811167, 5.379408587037500133 ) ) ;
#8553 = CARTESIAN_POINT ( 'NONE',  ( -0.2023972492402590084, -2.146007489747939978, 2.355265251465770149 ) ) ;
#8554 = ORIENTED_EDGE ( 'NONE', *, *, #4173, .F. ) ;
#8555 = VECTOR ( 'NONE', #344, 1000.000000000000000 ) ;
#8556 = DIRECTION ( 'NONE',  ( 0.7071067811865480168, 0.7071067811865470176, 0.000000000000000000 ) ) ;
#8557 = ORIENTED_EDGE ( 'NONE', *, *, #8952, .T. ) ;
#8558 = CARTESIAN_POINT ( 'NONE',  ( -1.962536940652958695, -2.895073591333140683, 5.998920491814799583 ) ) ;
#8559 = PRODUCT_CONTEXT ( 'NONE', #10890, 'mechanical' ) ;
#8560 = CARTESIAN_POINT ( 'NONE',  ( -2.230812463554230352, -5.497669491525425833, 6.137473736419926773 ) ) ;
#8561 = VERTEX_POINT ( 'NONE', #5666 ) ;
#8562 = CARTESIAN_POINT ( 'NONE',  ( -1.197297565406129971, -1.517223705964160008, 6.726135293448209929 ) ) ;
#8563 = CARTESIAN_POINT ( 'NONE',  ( -2.030998484741458832, -0.5180084745762725262, 4.999543428097190656 ) ) ;
#8564 = ORIENTED_EDGE ( 'NONE', *, *, #17947, .F. ) ;
#8565 = CARTESIAN_POINT ( 'NONE',  ( -1.550000000000000044, -5.599999999999999645, 5.100000000000000533 ) ) ;
#8566 = CARTESIAN_POINT ( 'NONE',  ( -1.889999999999999902, 7.299999999999999822, 1.327597122149119839E-15 ) ) ;
#8567 = AXIS2_PLACEMENT_3D ( 'NONE', #3848, #8368, #12807 ) ;
#8568 = CARTESIAN_POINT ( 'NONE',  ( 0.1086361371091010830, -2.937809291549738688, 6.750146344128172160 ) ) ;
#8569 = CARTESIAN_POINT ( 'NONE',  ( 1.399999999999999911, 0.5999999999999999778, 3.299999999999999822 ) ) ;
#8570 = VERTEX_POINT ( 'NONE', #1765 ) ;
#8571 = DIRECTION ( 'NONE',  ( 0.000000000000000000, 0.000000000000000000, -1.000000000000000000 ) ) ;
#8572 = VERTEX_POINT ( 'NONE', #189 ) ;
#8573 = DIRECTION ( 'NONE',  ( 6.123233995736823968E-17, 0.000000000000000000, 1.000000000000000000 ) ) ;
#8574 = CARTESIAN_POINT ( 'NONE',  ( 1.811729841638690219, -5.341949152542369461, 3.197954009834290012 ) ) ;
#8575 = EDGE_CURVE ( 'NONE', #10130, #14528, #11306, .T. ) ;
#8576 = CARTESIAN_POINT ( 'NONE',  ( 0.8570167067220199053, -0.01779661016949179650, 2.508190348879350218 ) ) ;
#8577 = EDGE_CURVE ( 'NONE', #10029, #4545, #14267, .T. ) ;
#8578 = CARTESIAN_POINT ( 'NONE',  ( 0.2812789908084389889, -5.444279661016950378, 7.036533610117280624 ) ) ;
#8579 = AXIS2_PLACEMENT_3D ( 'NONE', #7964, #3590, #17924 ) ;
#8580 = CARTESIAN_POINT ( 'NONE',  ( -0.5921572875253819923, 6.450000000000000178, 1.600000000000000089 ) ) ;
#8581 = EDGE_CURVE ( 'NONE', #13271, #14130, #7060, .T. ) ;
#8582 = ORIENTED_EDGE ( 'NONE', *, *, #1112, .F. ) ;
#8583 = LINE ( 'NONE', #9968, #5820 ) ;
#8584 = CARTESIAN_POINT ( 'NONE',  ( 1.460675875430079929, -0.9155690868286359141, 6.545310725710029587 ) ) ;
#8585 = DIRECTION ( 'NONE',  ( 0.000000000000000000, 1.000000000000000000, 0.000000000000000000 ) ) ;
#8586 = CARTESIAN_POINT ( 'NONE',  ( 1.992092870331701349, -2.196424942684489956, 4.203544726484164329 ) ) ;
#8587 = LINE ( 'NONE', #15260, #5825 ) ;
#8588 = VERTEX_POINT ( 'NONE', #104 ) ;
#8589 = AXIS2_PLACEMENT_3D ( 'NONE', #10895, #7830, #1076 ) ;
#8590 = EDGE_CURVE ( 'NONE', #13297, #13575, #5749, .T. ) ;
#8591 = DIRECTION ( 'NONE',  ( 0.000000000000000000, -1.000000000000000000, 0.000000000000000000 ) ) ;
#8592 = CARTESIAN_POINT ( 'NONE',  ( 2.268288188848061715, -0.04894067796610205440, 3.322421079292310786 ) ) ;
#8593 = CARTESIAN_POINT ( 'NONE',  ( 0.8189529353761060282, -3.822764246504690266, 2.493631540942729874 ) ) ;
#8594 = DIRECTION ( 'NONE',  ( 0.000000000000000000, 6.123233995736769734E-17, -1.000000000000000000 ) ) ;
#8595 = DIRECTION ( 'NONE',  ( 0.000000000000000000, 1.000000000000000000, 0.000000000000000000 ) ) ;
#8596 = CARTESIAN_POINT ( 'NONE',  ( -2.540842781840720654, -5.211016949152535993, 5.466141598148674952 ) ) ;
#8597 = ORIENTED_EDGE ( 'NONE', *, *, #14365, .T. ) ;
#8598 = ADVANCED_FACE ( 'NONE', ( #1394 ), #12702, .T. ) ;
#8599 = EDGE_LOOP ( 'NONE', ( #1018, #4632, #845, #11955 ) ) ;
#8600 = CARTESIAN_POINT ( 'NONE',  ( -2.318251751302029984, -5.233262711864408168, 4.294764266799000474 ) ) ;
#8601 = EDGE_CURVE ( 'NONE', #9483, #3235, #7319, .T. ) ;
#8602 = CARTESIAN_POINT ( 'NONE',  ( 1.588044008096809900, -0.7645959921354850142, 3.097578792715899976 ) ) ;
#8603 = EDGE_LOOP ( 'NONE', ( #11131, #7253, #12104, #597 ) ) ;
#8604 = B_SPLINE_CURVE_WITH_KNOTS ( 'NONE', 3,
 ( #2317, #2584, #12219, #15001, #6750, #12308, #1103, #7969, #17932, #16659, #16574, #9444, #3965, #15106, #16740, #6930 ),
 .UNSPECIFIED., .F., .F.,
 ( 4, 1, 1, 1, 1, 1, 1, 1, 1, 1, 1, 1, 1, 4 ),
 ( 0.4999998212288440103, 0.5105793490764080067, 0.5531463519625079428, 0.5957147871422280305, 0.6382850093032239602, 0.6808567369985039086, 0.7234300338917989404, 0.7660011046592689610, 0.8085801951441730084, 0.8511153557612559650, 0.8935297551199039567, 0.9363130006848809916, 0.9717764100585750686, 1.000000000000000000 ),
 .UNSPECIFIED. ) ;
#8605 = VECTOR ( 'NONE', #14595, 1000.000000000000000 ) ;
#8606 = CARTESIAN_POINT ( 'NONE',  ( -2.358786130709981332, -1.656953435693890864, 5.916240799583737164 ) ) ;
#8607 = CARTESIAN_POINT ( 'NONE',  ( 0.8469861386668179337, -0.7068739681193977331, 2.826929786773349385 ) ) ;
#8608 = EDGE_CURVE ( 'NONE', #16406, #14528, #8883, .T. ) ;
#8609 = CARTESIAN_POINT ( 'NONE',  ( 1.661700935788380074, -5.337500000000000355, 3.038299064211610112 ) ) ;
#8610 = CARTESIAN_POINT ( 'NONE',  ( 1.750000000000000000, 11.40000000000000036, 7.599999999999999645 ) ) ;
#8611 = CARTESIAN_POINT ( 'NONE',  ( 0.5320716618284230259, -2.592325843585389755, 6.992519451207130032 ) ) ;
#8612 = FACE_OUTER_BOUND ( 'NONE', #9412, .T. ) ;
#8613 = CARTESIAN_POINT ( 'NONE',  ( -1.460675875430050175, -4.684430913171359734, 6.545310725710059785 ) ) ;
#8614 = LINE ( 'NONE', #4334, #12902 ) ;
#8615 = CARTESIAN_POINT ( 'NONE',  ( 1.019987577504959608, -2.821367850108300157, 6.481720287913791623 ) ) ;
#8616 = DIRECTION ( 'NONE',  ( 5.421010862427519212E-16, 1.000000000000000000, 0.000000000000000000 ) ) ;
#8617 = VECTOR ( 'NONE', #13724, 1000.000000000000000 ) ;
#8618 = CARTESIAN_POINT ( 'NONE',  ( 1.750316316486830059, -0.3400423728813560253, 3.126818518378580158 ) ) ;
#8619 = VERTEX_POINT ( 'NONE', #9148 ) ;
#8620 = CARTESIAN_POINT ( 'NONE',  ( -0.4058874503045720172, 7.799999999999999822, 6.100000000000000533 ) ) ;
#8621 = ORIENTED_EDGE ( 'NONE', *, *, #14460, .T. ) ;
#8622 = EDGE_CURVE ( 'NONE', #10043, #1106, #16195, .T. ) ;
#8623 = DIRECTION ( 'NONE',  ( 1.480297366166879989E-15, 2.476791224480679883E-30, 1.000000000000000000 ) ) ;
#8624 = VERTEX_POINT ( 'NONE', #7678 ) ;
#8625 = DIRECTION ( 'NONE',  ( -1.000000000000000000, 2.843808977011158816E-15, -3.554761221263948421E-15 ) ) ;
#8626 = ORIENTED_EDGE ( 'NONE', *, *, #14858, .T. ) ;
#8627 = CARTESIAN_POINT ( 'NONE',  ( 1.562863241354470523, -5.408686440677975327, 6.031217337312382298 ) ) ;
#8628 = CARTESIAN_POINT ( 'NONE',  ( 1.889999999999999902, 3.500000000000000000, 0.6099999999999999867 ) ) ;
#8629 = CARTESIAN_POINT ( 'NONE',  ( -2.500000000000000000, 10.00000000000000000, 0.5999999999999999778 ) ) ;
#8630 = PLANE ( 'NONE',  #12601 ) ;
#8631 = DIRECTION ( 'NONE',  ( 0.000000000000000000, 0.000000000000000000, -1.000000000000000000 ) ) ;
#8632 = DIRECTION ( 'NONE',  ( 0.000000000000000000, 0.000000000000000000, 1.000000000000000000 ) ) ;
#8633 = CARTESIAN_POINT ( 'NONE',  ( -0.6343239990445920240, -2.099430913171359769, 2.433641963034089972 ) ) ;
#8634 = CARTESIAN_POINT ( 'NONE',  ( -1.181710496343089556, -2.801920438179980710, 6.378827610405741311 ) ) ;
#8635 = CARTESIAN_POINT ( 'NONE',  ( -2.350067830300900162, -0.2224576271186440024, 4.825253242917699303 ) ) ;
#8636 = LINE ( 'NONE', #7168, #3458 ) ;
#8637 = CARTESIAN_POINT ( 'NONE',  ( 2.350542563031990273, -1.004881363621820123, 4.817027120179740329 ) ) ;
#8638 = ORIENTED_EDGE ( 'NONE', *, *, #2702, .T. ) ;
#8639 = EDGE_CURVE ( 'NONE', #16536, #15044, #728, .T. ) ;
#8640 = CARTESIAN_POINT ( 'NONE',  ( -1.112838723655040107, -0.1735169491525430097, 6.773667561836210105 ) ) ;
#8641 = CARTESIAN_POINT ( 'NONE',  ( 0.2365712905368450025, -2.192584066324519743, 2.358466376073659720 ) ) ;
#8642 = EDGE_LOOP ( 'NONE', ( #9330, #1762, #6989, #2020 ) ) ;
#8643 = ORIENTED_EDGE ( 'NONE', *, *, #3137, .F. ) ;
#8644 = CARTESIAN_POINT ( 'NONE',  ( 1.552749016687789974, -4.036199717459258984, 6.468535037441731639 ) ) ;
#8645 = APPLICATION_PROTOCOL_DEFINITION ( 'draft international standard', 'automotive_design', 1998, #5912 ) ;
#8646 = CARTESIAN_POINT ( 'NONE',  ( -2.130266475405059090, -5.555508474576275724, 3.117337770017961418 ) ) ;
#8647 = VERTEX_POINT ( 'NONE', #4885 ) ;
#8648 = ADVANCED_FACE ( 'NONE', ( #16291 ), #10444, .F. ) ;
#8649 = CARTESIAN_POINT ( 'NONE',  ( -0.2453710345350140487, -0.4557203389830515317, 6.738252723719333481 ) ) ;
#8650 = VERTEX_POINT ( 'NONE', #11758 ) ;
#8651 = DIRECTION ( 'NONE',  ( -3.042833474898580443E-15, 3.289549702593060178E-16, 1.000000000000000000 ) ) ;
#8652 = CARTESIAN_POINT ( 'NONE',  ( -0.1749999999999999889, 7.700000000000000178, 0.4000000000000000222 ) ) ;
#8653 = CARTESIAN_POINT ( 'NONE',  ( 0.4874850653660255384, -2.891232714973161144, 6.694306935672937442 ) ) ;
#8654 = EDGE_LOOP ( 'NONE', ( #17139, #9582, #16737, #14534 ) ) ;
#8655 = CARTESIAN_POINT ( 'NONE',  ( -7.347880794884118997E-17, 0.5999999999999999778, 3.673940397442059498E-17 ) ) ;
#8656 = ORIENTED_EDGE ( 'NONE', *, *, #5692, .F. ) ;
#8657 = LINE ( 'NONE', #14307, #12158 ) ;
#8658 = CARTESIAN_POINT ( 'NONE',  ( 2.043308330018790198, -5.399788135593220240, 5.867646457774659652 ) ) ;
#8659 = AXIS2_PLACEMENT_3D ( 'NONE', #8838, #10312, #10574 ) ;
#8660 = CARTESIAN_POINT ( 'NONE',  ( -1.112838723655039885, -0.1735169491525430097, 6.773667561836209217 ) ) ;
#8661 = DIRECTION ( 'NONE',  ( -4.177994306516050823E-17, 0.7310552682428690385, -0.6823182503600111470 ) ) ;
#8662 = EDGE_CURVE ( 'NONE', #15551, #2515, #13259, .T. ) ;
#8663 = VERTEX_POINT ( 'NONE', #3597 ) ;
#8664 = DIRECTION ( 'NONE',  ( 0.000000000000000000, -1.000000000000000000, 0.000000000000000000 ) ) ;
#8665 = CARTESIAN_POINT ( 'NONE',  ( 0.08304008649498713368, -2.638902420161969520, 6.751342532748487280 ) ) ;
#8666 = LINE ( 'NONE', #3107, #8502 ) ;
#8667 = AXIS2_PLACEMENT_3D ( 'NONE', #9702, #15369, #8411 ) ;
#8668 = ORIENTED_EDGE ( 'NONE', *, *, #5774, .F. ) ;
#8669 = EDGE_CURVE ( 'NONE', #6244, #15780, #12385, .T. ) ;
#8670 = PLANE ( 'NONE',  #7365 ) ;
#8671 = CARTESIAN_POINT ( 'NONE',  ( 2.540842781840729536, -0.3889830508474575455, 5.466141598148674952 ) ) ;
#8672 = CARTESIAN_POINT ( 'NONE',  ( -1.661700935788390066, -0.5625000000000000000, 3.038299064211610112 ) ) ;
#8673 = DIRECTION ( 'NONE',  ( -1.000000000000000000, 2.220446049250315053E-16, 6.049014748177260544E-16 ) ) ;
#8674 = CARTESIAN_POINT ( 'NONE',  ( 1.000000000000000000, -6.000000000000000000, 3.673738709727309981 ) ) ;
#8675 = CARTESIAN_POINT ( 'NONE',  ( -1.973760952634090238, -5.259957627118655665, 2.925986839873730982 ) ) ;
#8676 = ORIENTED_EDGE ( 'NONE', *, *, #5942, .T. ) ;
#8677 = ORIENTED_EDGE ( 'NONE', *, *, #11291, .T. ) ;
#8678 = DIRECTION ( 'NONE',  ( 6.049014748177260544E-16, -2.493473113004680074E-16, 1.000000000000000000 ) ) ;
#8679 = LINE ( 'NONE', #18191, #12663 ) ;
#8680 = ORIENTED_EDGE ( 'NONE', *, *, #6412, .F. ) ;
#8681 = VECTOR ( 'NONE', #12527, 1000.000000000000000 ) ;
#8682 = EDGE_CURVE ( 'NONE', #9295, #12680, #14532, .T. ) ;
#8683 = CARTESIAN_POINT ( 'NONE',  ( -0.4247583764260595141, -1.424070552811000701, 7.319674410047512403 ) ) ;
#8684 = EDGE_CURVE ( 'NONE', #5295, #7602, #3400, .T. ) ;
#8685 = CARTESIAN_POINT ( 'NONE',  ( 1.458615186838411626, -0.4963798976394455664, 3.259477383973563125 ) ) ;
#8686 = DIRECTION ( 'NONE',  ( 1.000000000000000000, 0.000000000000000000, 0.000000000000000000 ) ) ;
#8687 = CARTESIAN_POINT ( 'NONE',  ( 0.6918414964981909332, -1.940253771513320125, 2.450533167346750307 ) ) ;
#8688 = EDGE_CURVE ( 'NONE', #13417, #2212, #9241, .T. ) ;
#8689 = EDGE_CURVE ( 'NONE', #2121, #7170, #14905, .T. ) ;
#8690 = CARTESIAN_POINT ( 'NONE',  ( 1.732245706108171746, -5.033893599512585304, 2.684512698446369861 ) ) ;
#8691 = CARTESIAN_POINT ( 'NONE',  ( 0.8001094918299610503, -1.307629111369559949, 7.230402832373829192 ) ) ;
#8692 = STYLED_ITEM ( 'NONE', ( #14068 ), #1903 ) ;
#8693 = ADVANCED_FACE ( 'NONE', ( #6098 ), #3325, .T. ) ;
#8694 = DIRECTION ( 'NONE',  ( 0.000000000000000000, -1.000000000000000000, 0.000000000000000000 ) ) ;
#8695 = EDGE_CURVE ( 'NONE', #14203, #1528, #14810, .T. ) ;
#8696 = CARTESIAN_POINT ( 'NONE',  ( -1.417606053559450352, -4.707719201459645397, 6.185023541745952258 ) ) ;
#8697 = LINE ( 'NONE', #1661, #1958 ) ;
#8698 = ADVANCED_FACE ( 'NONE', ( #1930 ), #7497, .T. ) ;
#8699 = CARTESIAN_POINT ( 'NONE',  ( 1.550000000000000044, -5.599999999999999645, 6.100000000000000533 ) ) ;
#8700 = ORIENTED_EDGE ( 'NONE', *, *, #10764, .T. ) ;
#8701 = DIRECTION ( 'NONE',  ( -1.264200168623419965E-31, -8.540177112501209562E-17, 1.000000000000000000 ) ) ;
#8702 = ORIENTED_EDGE ( 'NONE', *, *, #1240, .F. ) ;
#8703 = DIRECTION ( 'NONE',  ( -1.853875224168160112E-15, -1.000000000000000000, -2.960594732333760372E-15 ) ) ;
#8704 = ORIENTED_EDGE ( 'NONE', *, *, #6448, .T. ) ;
#8705 = CARTESIAN_POINT ( 'NONE',  ( -0.3803919826357066158, -5.591101694915256104, 2.682580100125310896 ) ) ;
#8706 = LINE ( 'NONE', #8971, #11508 ) ;
#8707 = CARTESIAN_POINT ( 'NONE',  ( -0.8642983280852033490, -2.732055573315119723, 7.209203477813437289 ) ) ;
#8708 = FILL_AREA_STYLE ('',( #10447 ) ) ;
#8709 = FACE_OUTER_BOUND ( 'NONE', #5069, .T. ) ;
#8710 = CARTESIAN_POINT ( 'NONE',  ( -0.2109711709854041328, -5.280843314568215874, 2.050669023674909663 ) ) ;
#8711 = EDGE_CURVE ( 'NONE', #14368, #6950, #15931, .T. ) ;
#8712 = CARTESIAN_POINT ( 'NONE',  ( 0.03000000000000110217, 11.40000000000000036, 1.600000000000000089 ) ) ;
#8713 = LINE ( 'NONE', #9922, #12974 ) ;
#8714 = CARTESIAN_POINT ( 'NONE',  ( 1.265407828724300021, -2.309025507765960050, 2.715689360385540319 ) ) ;
#8715 = CARTESIAN_POINT ( 'NONE',  ( -1.138568046961029978, -4.362235753495300905, 6.408380708468528475 ) ) ;
#8716 = CARTESIAN_POINT ( 'NONE',  ( -1.477796163681079911, -0.1824152542372889929, 6.531563725478150673 ) ) ;
#8717 = CARTESIAN_POINT ( 'NONE',  ( -1.399999999999999911, 0.5999999999999999778, 6.100000000000000533 ) ) ;
#8718 = CARTESIAN_POINT ( 'NONE',  ( -1.500000000000000000, -5.599999999999999645, 2.299999999999999822 ) ) ;
#8719 = VERTEX_POINT ( 'NONE', #11936 ) ;
#8720 = CARTESIAN_POINT ( 'NONE',  ( -0.3162622016569221484, -4.245794312053864594, 7.334974746141788238 ) ) ;
#8721 = CARTESIAN_POINT ( 'NONE',  ( 2.041338374031088865, -0.08008474576271226719, 4.918217215283659627 ) ) ;
#8722 = CARTESIAN_POINT ( 'NONE',  ( -2.340959815966380031, -1.750106588847040179, 4.942183458383479611 ) ) ;
#8723 = ORIENTED_EDGE ( 'NONE', *, *, #6527, .F. ) ;
#8724 = CARTESIAN_POINT ( 'NONE',  ( 0.9000000000000000222, -10.00000000000000000, 3.799999999999999822 ) ) ;
#8725 = ORIENTED_EDGE ( 'NONE', *, *, #1005, .T. ) ;
#8726 = CARTESIAN_POINT ( 'NONE',  ( 0.5902886515193200845, -4.152641158900700624, 6.978224088050040130 ) ) ;
#8727 = SHAPE_DEFINITION_REPRESENTATION ( #6843, #8322 ) ;
#8728 = CARTESIAN_POINT ( 'NONE',  ( -1.347262683220810553, -5.175423728813555613, 6.986424775243341045 ) ) ;
#8729 = ORIENTED_EDGE ( 'NONE', *, *, #2012, .T. ) ;
#8730 = LINE ( 'NONE', #11687, #7909 ) ;
#8731 = CARTESIAN_POINT ( 'NONE',  ( 0.1365430262726380628, -0.4468220338983063811, 6.748423079423377047 ) ) ;
#8732 = EDGE_LOOP ( 'NONE', ( #6192, #10496, #1445, #8031 ) ) ;
#8733 = EDGE_CURVE ( 'NONE', #14961, #16021, #17650, .T. ) ;
#8734 = LINE ( 'NONE', #16975, #12913 ) ;
#8735 = DIRECTION ( 'NONE',  ( 0.000000000000000000, 0.000000000000000000, 1.000000000000000000 ) ) ;
#8736 = CARTESIAN_POINT ( 'NONE',  ( -0.5549238885286955636, -2.099430913171361102, 2.723396519134838822 ) ) ;
#8737 = DIRECTION ( 'NONE',  ( 1.224646799147350002E-16, -1.000000000000000000, -6.123233995736769734E-17 ) ) ;
#8738 = CARTESIAN_POINT ( 'NONE',  ( 1.192209327851080136, -0.3222457627118649470, 2.329031440774910422 ) ) ;
#8739 = EDGE_LOOP ( 'NONE', ( #11161, #499, #17769, #9552 ) ) ;
#8740 = LINE ( 'NONE', #14384, #220 ) ;
#8741 = CARTESIAN_POINT ( 'NONE',  ( 1.626487163628800081, -5.044101657174960174, 3.073512836371200319 ) ) ;
#8742 = ORIENTED_EDGE ( 'NONE', *, *, #2751, .F. ) ;
#8743 = DIRECTION ( 'NONE',  ( -1.000000000000000000, 3.700743415417190112E-16, 7.273661547324619914E-16 ) ) ;
#8744 = CARTESIAN_POINT ( 'NONE',  ( 1.641808337277750107, -5.413135593220339103, 6.386111670537619744 ) ) ;
#8745 = APPLICATION_CONTEXT ( 'automotive_design' ) ;
#8746 = VECTOR ( 'NONE', #9485, 1000.000000000000000 ) ;
#8747 = PLANE ( 'NONE',  #17155 ) ;
#8748 = CARTESIAN_POINT ( 'NONE',  ( 0.009452110982654814836, -0.3001920447045380858, 2.649999999999998579 ) ) ;
#8749 = ORIENTED_EDGE ( 'NONE', *, *, #7009, .F. ) ;
#8750 = CARTESIAN_POINT ( 'NONE',  ( -1.550000000000000044, -6.000000000000000000, 5.100000000000000533 ) ) ;
#8751 = CARTESIAN_POINT ( 'NONE',  ( -0.1768565782246520057, -1.847100618360170143, 2.353200596935780098 ) ) ;
#8752 = CIRCLE ( 'NONE', #4015, 0.09999999999999939493 ) ;
#8753 = CARTESIAN_POINT ( 'NONE',  ( -1.899999999999999911, 7.299999999999999822, 0.5999999999999999778 ) ) ;
#8754 = CARTESIAN_POINT ( 'NONE',  ( -1.599895119336340876, -2.871785303044851023, 5.986560317183706736 ) ) ;
#8755 = AXIS2_PLACEMENT_3D ( 'NONE', #9626, #12321, #17847 ) ;
#8756 = DIRECTION ( 'NONE',  ( -5.551115123125780730E-16, -1.000000000000000000, 0.000000000000000000 ) ) ;
#8757 = TOROIDAL_SURFACE ( 'NONE', #16784, 0.2999999999999999889, 0.2500000000000000000 ) ;
#8758 = ORIENTED_EDGE ( 'NONE', *, *, #8918, .T. ) ;
#8759 = VECTOR ( 'NONE', #15111, 1000.000000000000227 ) ;
#8760 = EDGE_CURVE ( 'NONE', #18244, #10646, #8541, .T. ) ;
#8761 = LINE ( 'NONE', #346, #10591 ) ;
#8762 = CARTESIAN_POINT ( 'NONE',  ( 1.610878918935058524, -0.03114406779661053892, 2.590989782159081933 ) ) ;
#8763 = CARTESIAN_POINT ( 'NONE',  ( -1.282210379528740063, -4.661142624883069630, 6.673494927815290190 ) ) ;
#8764 = DIRECTION ( 'NONE',  ( 1.000000000000000000, 0.000000000000000000, 0.000000000000000000 ) ) ;
#8765 = CARTESIAN_POINT ( 'NONE',  ( -0.5372984490435469551, 4.599999999999999645, 8.300000000000000711 ) ) ;
#8766 = CARTESIAN_POINT ( 'NONE',  ( 1.925796468768800063, -5.104237288135590411, 6.052706598917719560 ) ) ;
#8767 = EDGE_LOOP ( 'NONE', ( #7357, #3844, #12593, #15204, #1155, #15124, #2773, #702 ) ) ;
#8768 = EDGE_LOOP ( 'NONE', ( #16063, #4231, #790, #17871 ) ) ;
#8769 = DIRECTION ( 'NONE',  ( 2.220446049250309876E-16, 1.000000000000000000, -5.551115123125800057E-15 ) ) ;
#8770 = DIRECTION ( 'NONE',  ( -9.349246523159200620E-16, 0.000000000000000000, 1.000000000000000000 ) ) ;
#8771 = ORIENTED_EDGE ( 'NONE', *, *, #14236, .T. ) ;
#8772 = VECTOR ( 'NONE', #11248, 1000.000000000000000 ) ;
#8773 = CARTESIAN_POINT ( 'NONE',  ( 2.584100759211419795, -0.9350164987569505870, 4.095403473953104445 ) ) ;
#8774 = DIRECTION ( 'NONE',  ( -1.480297366166879989E-15, -1.000000000000000000, 1.314768175368350090E-30 ) ) ;
#8775 = CARTESIAN_POINT ( 'NONE',  ( 0.7500000000000000000, 3.050000000000000266, 3.200000000000000178 ) ) ;
#8776 = CARTESIAN_POINT ( 'NONE',  ( -1.567709126316399804, -1.684082600342149849, 2.944712621036610134 ) ) ;
#8777 = AXIS2_PLACEMENT_3D ( 'NONE', #16717, #1081, #13483 ) ;
#8778 = DIRECTION ( 'NONE',  ( -1.000000000000000000, 4.906538933386810061E-16, 0.000000000000000000 ) ) ;
#8779 = CARTESIAN_POINT ( 'NONE',  ( 0.06913820924143311564, -1.377493976234431372, 7.352985789827153340 ) ) ;
#8780 = DIRECTION ( 'NONE',  ( -1.000000000000000000, 0.000000000000000000, 1.048990684667790150E-15 ) ) ;
#8781 = FACE_OUTER_BOUND ( 'NONE', #3356, .T. ) ;
#8782 = CARTESIAN_POINT ( 'NONE',  ( 1.652654650382400003, -0.7952867690272209522, 3.029252778805620050 ) ) ;
#8783 = AXIS2_PLACEMENT_3D ( 'NONE', #12840, #4037, #2566 ) ;
#8784 = CARTESIAN_POINT ( 'NONE',  ( 1.899999999999999911, 11.40000000000000036, 1.600000000000000089 ) ) ;
#8785 = VECTOR ( 'NONE', #1505, 1000.000000000000000 ) ;
#8786 = CIRCLE ( 'NONE', #2875, 0.3499999999999996447 ) ;
#8787 = DIRECTION ( 'NONE',  ( 1.000000000000000000, -1.480297366166879989E-15, 0.000000000000000000 ) ) ;
#8788 = EDGE_LOOP ( 'NONE', ( #3835, #7152, #7924, #3656 ) ) ;
#8789 = ADVANCED_FACE ( 'NONE', ( #457, #4608 ), #10263, .T. ) ;
#8790 = VERTEX_POINT ( 'NONE', #18024 ) ;
#8791 = DIRECTION ( 'NONE',  ( -1.142385477618690234E-14, 1.110223024625159992E-16, -1.000000000000000000 ) ) ;
#8792 = CIRCLE ( 'NONE', #9077, 0.2500000000000002220 ) ;
#8793 = EDGE_CURVE ( 'NONE', #13096, #16755, #4054, .T. ) ;
#8794 = AXIS2_PLACEMENT_3D ( 'NONE', #15318, #18055, #8449 ) ;
#8795 = ORIENTED_EDGE ( 'NONE', *, *, #15544, .F. ) ;
#8796 = EDGE_CURVE ( 'NONE', #5515, #16687, #5275, .T. ) ;
#8797 = CARTESIAN_POINT ( 'NONE',  ( 1.432215783582721613, -5.413135593220339992, 6.170863372171116801 ) ) ;
#8798 = ADVANCED_FACE ( 'NONE', ( #17753 ), #1017, .T. ) ;
#8799 = CARTESIAN_POINT ( 'NONE',  ( -1.094547058713670085, -2.755343861603408939, 7.117660114503937763 ) ) ;
#8800 = VECTOR ( 'NONE', #15872, 1000.000000000000000 ) ;
#8801 = CARTESIAN_POINT ( 'NONE',  ( 4.898587196589409994E-17, 0.1000000000000000056, 8.300000000000000711 ) ) ;
#8802 = VECTOR ( 'NONE', #5155, 1000.000000000000000 ) ;
#8803 = CARTESIAN_POINT ( 'NONE',  ( 1.875000000000000000, 0.7500000000000000000, 7.700000000000000178 ) ) ;
#8804 = CARTESIAN_POINT ( 'NONE',  ( 2.331386066015260106, -0.9583047870452390260, 4.378465089518139841 ) ) ;
#8805 = DIRECTION ( 'NONE',  ( -2.337311630789800155E-16, 1.000000000000000000, 1.168655815394900078E-16 ) ) ;
#8806 = CARTESIAN_POINT ( 'NONE',  ( -2.159566522375440112, -3.240557039297490061, 5.635424033751089468 ) ) ;
#8807 =( GEOMETRIC_REPRESENTATION_CONTEXT ( 3 ) GLOBAL_UNCERTAINTY_ASSIGNED_CONTEXT ( ( #13636 ) ) GLOBAL_UNIT_ASSIGNED_CONTEXT ( ( #2591, #12774, #9994 ) ) REPRESENTATION_CONTEXT ( 'NONE', 'WORKASPACE' ) );
#8808 = CARTESIAN_POINT ( 'NONE',  ( 1.203420131881999477, -4.059488005747546424, 6.363334551077796775 ) ) ;
#8809 = TOROIDAL_SURFACE ( 'NONE', #2608, 0.2999999999999999889, 0.2500000000000000000 ) ;
#8810 = CARTESIAN_POINT ( 'NONE',  ( 2.253200202764420013, -0.3889830508474579895, 5.379408587037500133 ) ) ;
#8811 = DIRECTION ( 'NONE',  ( -0.000000000000000000, 1.000000000000000000, 0.000000000000000000 ) ) ;
#8812 = DIRECTION ( 'NONE',  ( -1.000000000000000000, 0.000000000000000000, 0.000000000000000000 ) ) ;
#8813 = ORIENTED_EDGE ( 'NONE', *, *, #7004, .F. ) ;
#8814 = CARTESIAN_POINT ( 'NONE',  ( 0.4247583764261176897, -4.175929447188994281, 7.319674410047496416 ) ) ;
#8815 = VECTOR ( 'NONE', #64, 1000.000000000000000 ) ;
#8816 = CARTESIAN_POINT ( 'NONE',  ( 0.1910247150515120007, -0.3044491525423730915, 2.655937705488500722 ) ) ;
#8817 = CARTESIAN_POINT ( 'NONE',  ( 0.01716182025089369942, -2.169295778036230082, 2.346608583467340026 ) ) ;
#8818 = VECTOR ( 'NONE', #3148, 1000.000000000000000 ) ;
#8819 = EDGE_LOOP ( 'NONE', ( #10820, #8053, #14023, #4635 ) ) ;
#8820 = ORIENTED_EDGE ( 'NONE', *, *, #13839, .F. ) ;
#8821 = FACE_OUTER_BOUND ( 'NONE', #285, .T. ) ;
#8822 = EDGE_CURVE ( 'NONE', #9265, #16382, #11011, .T. ) ;
#8823 = ORIENTED_EDGE ( 'NONE', *, *, #4820, .F. ) ;
#8824 = CARTESIAN_POINT ( 'NONE',  ( 1.586727176531399941, -3.617010528270070413, 2.961885344765600614 ) ) ;
#8825 = VECTOR ( 'NONE', #3029, 1000.000000000000000 ) ;
#8826 = APPLICATION_PROTOCOL_DEFINITION ( 'draft international standard', 'automotive_design', 1998, #2381 ) ;
#8827 = CARTESIAN_POINT ( 'NONE',  ( -2.638803263991410741, -5.219915254237295521, 4.982085668537435730 ) ) ;
#8828 = VECTOR ( 'NONE', #4523, 1000.000000000000000 ) ;
#8829 = ORIENTED_EDGE ( 'NONE', *, *, #11113, .F. ) ;
#8830 = PLANE ( 'NONE',  #15896 ) ;
#8831 = CARTESIAN_POINT ( 'NONE',  ( 1.851073041990159984, -0.4067796610169499560, 6.153284478378259870 ) ) ;
#8832 = VERTEX_POINT ( 'NONE', #1198 ) ;
#8833 = DIRECTION ( 'NONE',  ( 5.473822126269209268E-48, 1.000000000000000000, 1.332267629550190018E-15 ) ) ;
#8834 = CARTESIAN_POINT ( 'NONE',  ( -2.500000000000000000, 9.199999999999999289, 1.600000000000000089 ) ) ;
#8835 = CARTESIAN_POINT ( 'NONE',  ( 2.025702773739959106, -2.518620102360551893, 4.366188503657621567 ) ) ;
#8836 = CARTESIAN_POINT ( 'NONE',  ( 2.458531667407859889, -0.3934322033898309257, 5.699238225248945966 ) ) ;
#8837 = ORIENTED_EDGE ( 'NONE', *, *, #8608, .F. ) ;
#8838 = CARTESIAN_POINT ( 'NONE',  ( -1.899999999999999911, 9.199999999999999289, 1.600000000000000089 ) ) ;
#8839 = VECTOR ( 'NONE', #17797, 1000.000000000000000 ) ;
#8840 = DIRECTION ( 'NONE',  ( -1.224646799147350002E-16, 1.000000000000000000, 6.123233995736769734E-17 ) ) ;
#8841 = VECTOR ( 'NONE', #7243, 1000.000000000000000 ) ;
#8842 = ORIENTED_EDGE ( 'NONE', *, *, #6220, .F. ) ;
#8843 = CARTESIAN_POINT ( 'NONE',  ( -0.006659065580995300951, -0.5555405507507519269, 2.241023775284399999 ) ) ;
#8844 = CARTESIAN_POINT ( 'NONE',  ( -1.921786527979019166, -5.542161016949150643, 3.977907449687794195 ) ) ;
#8845 = DIRECTION ( 'NONE',  ( -1.000000000000000000, 0.000000000000000000, 0.000000000000000000 ) ) ;
#8846 = EDGE_CURVE ( 'NONE', #4727, #5712, #10734, .T. ) ;
#8847 = DIRECTION ( 'NONE',  ( 0.000000000000000000, 1.774290917998389804E-45, -1.000000000000000000 ) ) ;
#8848 = CARTESIAN_POINT ( 'NONE',  ( -2.649291707874080970, -3.356998480738929924, 4.543900225523854530 ) ) ;
#8849 = ORIENTED_EDGE ( 'NONE', *, *, #662, .F. ) ;
#8850 = AXIS2_PLACEMENT_3D ( 'NONE', #12631, #18258, #11250 ) ;
#8851 = CARTESIAN_POINT ( 'NONE',  ( -0.9719602541832299547, -2.755343861603410271, 6.843370931913550059 ) ) ;
#8852 = FACE_OUTER_BOUND ( 'NONE', #2792, .T. ) ;
#8853 = CARTESIAN_POINT ( 'NONE',  ( 2.035869680587130137, -2.289578095837640159, 4.964832940349494628 ) ) ;
#8854 = FACE_OUTER_BOUND ( 'NONE', #8768, .T. ) ;
#8855 = DIRECTION ( 'NONE',  ( -0.7071067811865470176, 0.7071067811865480168, 0.000000000000000000 ) ) ;
#8856 = ORIENTED_EDGE ( 'NONE', *, *, #3172, .T. ) ;
#8857 = FACE_OUTER_BOUND ( 'NONE', #6189, .T. ) ;
#8858 = VECTOR ( 'NONE', #5856, 1000.000000000000000 ) ;
#8859 = CARTESIAN_POINT ( 'NONE',  ( 2.311987889326980294, -4.078935417675859654, 4.260161748947079552 ) ) ;
#8860 = LINE ( 'NONE', #2085, #3948 ) ;
#8861 = CARTESIAN_POINT ( 'NONE',  ( 6.858022075225179538E-16, -5.000000000000000000, -3.061616997868380183E-16 ) ) ;
#8862 = CARTESIAN_POINT ( 'NONE',  ( -2.230812463554230352, -5.197669491525426011, 6.137473736419926773 ) ) ;
#8863 = ORIENTED_EDGE ( 'NONE', *, *, #9253, .F. ) ;
#8864 = ADVANCED_FACE ( 'NONE', ( #11095 ), #15278, .F. ) ;
#8865 = VERTEX_POINT ( 'NONE', #16380 ) ;
#8866 = DIRECTION ( 'NONE',  ( 1.000000000000000000, 0.000000000000000000, 0.000000000000000000 ) ) ;
#8867 = CARTESIAN_POINT ( 'NONE',  ( 1.899999999999999911, 11.29999999999999893, 1.600000000000000089 ) ) ;
#8868 = ORIENTED_EDGE ( 'NONE', *, *, #11413, .F. ) ;
#8869 = CARTESIAN_POINT ( 'NONE',  ( 0.02098813186351079427, -2.169295778036230526, 2.046196467083000403 ) ) ;
#8870 = CARTESIAN_POINT ( 'NONE',  ( 1.526064881623949931, -0.7763906680874419486, 2.903976516638540062 ) ) ;
#8871 = LINE ( 'NONE', #7300, #2309 ) ;
#8872 = VECTOR ( 'NONE', #17831, 1000.000000000000000 ) ;
#8873 = CARTESIAN_POINT ( 'NONE',  ( 1.917298190932609891, -2.103271789531340197, 3.335187436117899917 ) ) ;
#8874 = CARTESIAN_POINT ( 'NONE',  ( 1.468674196027861756, -1.237764246504700072, 6.910454658870847311 ) ) ;
#8875 = FACE_OUTER_BOUND ( 'NONE', #6499, .T. ) ;
#8876 = CARTESIAN_POINT ( 'NONE',  ( 1.632144308286169965, -4.288530012270460823, 5.945394234592866312 ) ) ;
#8877 = CARTESIAN_POINT ( 'NONE',  ( 1.250000000000000000, 0.5999999999999999778, 7.599999999999999645 ) ) ;
#8878 = ORIENTED_EDGE ( 'NONE', *, *, #15501, .T. ) ;
#8879 = DIRECTION ( 'NONE',  ( 2.220446049250309876E-16, 0.000000000000000000, -1.000000000000000000 ) ) ;
#8880 = ORIENTED_EDGE ( 'NONE', *, *, #4313, .T. ) ;
#8881 = LINE ( 'NONE', #4607, #13210 ) ;
#8882 = VECTOR ( 'NONE', #8999, 1000.000000000000000 ) ;
#8883 = LINE ( 'NONE', #4792, #4964 ) ;
#8884 = VERTEX_POINT ( 'NONE', #6654 ) ;
#8885 = CARTESIAN_POINT ( 'NONE',  ( 2.034805890357269220, -5.368644067796615182, 4.427518626519221456 ) ) ;
#8886 = DIRECTION ( 'NONE',  ( 6.123233995736768501E-17, 0.000000000000000000, 1.000000000000000000 ) ) ;
#8887 = SURFACE_SIDE_STYLE ('',( #17288 ) ) ;
#8888 = CARTESIAN_POINT ( 'NONE',  ( 2.234315482767910144, -5.359745762711869865, 3.960850823455320580 ) ) ;
#8889 = DIRECTION ( 'NONE',  ( 0.000000000000000000, 0.000000000000000000, 1.000000000000000000 ) ) ;
#8890 = CARTESIAN_POINT ( 'NONE',  ( 1.794646911016580137, -1.167899381639829981, 6.222494056560660347 ) ) ;
#8891 = CARTESIAN_POINT ( 'NONE',  ( 0.8740908734716299477, 4.154758922476410099, 8.300000000000000711 ) ) ;
#8892 = AXIS2_PLACEMENT_3D ( 'NONE', #7742, #10612, #6625 ) ;
#8893 = CARTESIAN_POINT ( 'NONE',  ( -0.6918414964982418924, -3.659746228486680408, 2.450533167346770291 ) ) ;
#8894 = CARTESIAN_POINT ( 'NONE',  ( -1.942813984510721070, -4.525253771513313872, 5.363608065214459764 ) ) ;
#8895 = EDGE_CURVE ( 'NONE', #13175, #14300, #8604, .T. ) ;
#8896 = CARTESIAN_POINT ( 'NONE',  ( -0.009452173233712278175, -5.299808941921980043, 2.358866582356820008 ) ) ;
#8897 = EDGE_CURVE ( 'NONE', #13468, #1492, #13615, .T. ) ;
#8898 = DIRECTION ( 'NONE',  ( -1.000000000000000000, 0.000000000000000000, 0.000000000000000000 ) ) ;
#8899 = ORIENTED_EDGE ( 'NONE', *, *, #14645, .F. ) ;
#8900 =( BOUNDED_SURFACE ( )  B_SPLINE_SURFACE ( 3, 3, ( 
 ( #16348, #15076, #6534, #2387, #14030, #1260, #16808 ),
 ( #6905, #12645, #8306, #5429, #18270, #11066, #18082 ),
 ( #8205, #13852, #9960, #1171, #7106, #6819, #11351 ),
 ( #4023, #10986, #12745, #12374, #2552, #15348, #12464 ),
 ( #60, #5616, #18162, #4298, #16710, #5706, #9677 ),
 ( #2653, #6997, #12553, #13943, #4121, #11260, #11159 ),
 ( #2932, #9780, #16984, #9588, #4209, #15441, #16634 ) ),
 .UNSPECIFIED., .T., .F., .F. ) 
 B_SPLINE_SURFACE_WITH_KNOTS ( ( 4, 3, 4 ),
 ( 4, 1, 1, 1, 4 ),
 ( 0.000000000000000000, 3.141592653589790007, 6.283185307179590673 ),
 ( 18.06415775814129887, 18.36448856483159986, 18.49670707487869947, 18.62179267666130045, 18.84955592153880133 ),
 .UNSPECIFIED. ) 
 GEOMETRIC_REPRESENTATION_ITEM ( )  RATIONAL_B_SPLINE_SURFACE ( (
 ( 1.000000000000000000, 1.000000000000000000, 1.000000000000000000, 1.000000000000000000, 1.000000000000000000, 1.000000000000000000, 1.000000000000000000),
 ( 0.3333333333333329818, 0.3333333333333329818, 0.3333333333333329818, 0.3333333333333329818, 0.3333333333333329818, 0.3333333333333329818, 0.3333333333333329818),
 ( 0.3333333333333329818, 0.3333333333333329818, 0.3333333333333329818, 0.3333333333333329818, 0.3333333333333329818, 0.3333333333333329818, 0.3333333333333329818),
 ( 1.000000000000000000, 1.000000000000000000, 1.000000000000000000, 1.000000000000000000, 1.000000000000000000, 1.000000000000000000, 1.000000000000000000),
 ( 0.3333333333333329818, 0.3333333333333329818, 0.3333333333333329818, 0.3333333333333329818, 0.3333333333333329818, 0.3333333333333329818, 0.3333333333333329818),
 ( 0.3333333333333329818, 0.3333333333333329818, 0.3333333333333329818, 0.3333333333333329818, 0.3333333333333329818, 0.3333333333333329818, 0.3333333333333329818),
 ( 1.000000000000000000, 1.000000000000000000, 1.000000000000000000, 1.000000000000000000, 1.000000000000000000, 1.000000000000000000, 1.000000000000000000) ) ) 
 REPRESENTATION_ITEM ( '' )  SURFACE ( )  );
#8901 = CARTESIAN_POINT ( 'NONE',  ( 1.901882987994760965, -0.09343220338983100615, 5.472995608211450147 ) ) ;
#8902 = CARTESIAN_POINT ( 'NONE',  ( 1.991984774470479946, -3.985782264522710339, 3.446707398186009907 ) ) ;
#8903 = ORIENTED_EDGE ( 'NONE', *, *, #6527, .T. ) ;
#8904 = ORIENTED_EDGE ( 'NONE', *, *, #3196, .F. ) ;
#8905 = CARTESIAN_POINT ( 'NONE',  ( -2.500000000000000000, 11.29999999999999893, 1.600000000000000089 ) ) ;
#8906 = VERTEX_POINT ( 'NONE', #8234 ) ;
#8907 = CARTESIAN_POINT ( 'NONE',  ( 2.005512128484128631, -3.686875393134939838, 3.468469736471341491 ) ) ;
#8908 = CARTESIAN_POINT ( 'NONE',  ( -8.358484336133781903E-17, -4.999999999999999112, -1.016439536705160407E-15 ) ) ;
#8909 = CARTESIAN_POINT ( 'NONE',  ( 2.191755591049679541, -5.046398305084744962, 3.203650300307709475 ) ) ;
#8910 = DIRECTION ( 'NONE',  ( -5.401922984254539957E-62, -1.000000000000000000, 1.836189155707839943E-31 ) ) ;
#8911 = CARTESIAN_POINT ( 'NONE',  ( -2.351526912647309953, -0.5269067796610169552, 4.606040641882809261 ) ) ;
#8912 = ORIENTED_EDGE ( 'NONE', *, *, #9347, .T. ) ;
#8913 = ADVANCED_FACE ( 'NONE', ( #2419 ), #6567, .T. ) ;
#8914 = DIRECTION ( 'NONE',  ( 1.000000000000000000, -1.445602896647339114E-15, 2.891205793294678228E-15 ) ) ;
#8915 = CYLINDRICAL_SURFACE ( 'NONE', #17073, 0.2500000000000002220 ) ;
#8916 = LINE ( 'NONE', #5845, #16818 ) ;
#8917 = CARTESIAN_POINT ( 'NONE',  ( -1.934380261529029754, -4.824160642901089702, 5.387804366397155320 ) ) ;
#8918 = EDGE_CURVE ( 'NONE', #11214, #9511, #9710, .T. ) ;
#8919 = CARTESIAN_POINT ( 'NONE',  ( -2.431060148753501515, -0.5447033898305090327, 3.635668498923334102 ) ) ;
#8920 = ORIENTED_EDGE ( 'NONE', *, *, #11096, .F. ) ;
#8921 = DIRECTION ( 'NONE',  ( 1.000000000000000000, 0.000000000000000000, 0.000000000000000000 ) ) ;
#8922 = EDGE_CURVE ( 'NONE', #15242, #18244, #17381, .T. ) ;
#8923 = FACE_OUTER_BOUND ( 'NONE', #2736, .T. ) ;
#8924 = EDGE_CURVE ( 'NONE', #2205, #15023, #11791, .T. ) ;
#8925 = VERTEX_POINT ( 'NONE', #13965 ) ;
#8926 = ADVANCED_FACE ( 'NONE', ( #1287 ), #17230, .F. ) ;
#8927 = LINE ( 'NONE', #1718, #2683 ) ;
#8928 = CARTESIAN_POINT ( 'NONE',  ( -2.293398556041709835, -0.2358050847457630328, 4.171956209133481863 ) ) ;
#8929 = CARTESIAN_POINT ( 'NONE',  ( -0.1926573868394080846, -0.2965485159365558454, 2.049233193116839935 ) ) ;
#8930 = CARTESIAN_POINT ( 'NONE',  ( 2.370419177058800120, -4.241953435693877061, 5.893409660608535994 ) ) ;
#8931 = ORIENTED_EDGE ( 'NONE', *, *, #761, .T. ) ;
#8932 = CARTESIAN_POINT ( 'NONE',  ( 1.816660071039059909, -2.429307825567370127, 6.196159040268200968 ) ) ;
#8933 = PLANE ( 'NONE',  #12940 ) ;
#8934 = CARTESIAN_POINT ( 'NONE',  ( 0.1749999999999999889, 7.500000000000000000, 1.600000000000000089 ) ) ;
#8935 = CARTESIAN_POINT ( 'NONE',  ( -0.8893259633308450152, -1.753947465207011058, 2.849594321892158888 ) ) ;
#8937 = EDGE_CURVE ( 'NONE', #8663, #5929, #15783, .T. ) ;
#8936 = CARTESIAN_POINT ( 'NONE',  ( -1.800000000000000044, 0.5999999999999999778, 7.550000000000000711 ) ) ;
#8938 = VERTEX_POINT ( 'NONE', #11692 ) ;
#8939 = LINE ( 'NONE', #16935, #5556 ) ;
#8940 = LINE ( 'NONE', #14237, #11788 ) ;
#8941 = CARTESIAN_POINT ( 'NONE',  ( -0.6919952253609726878, -1.148451969711520082, 7.262080463428013388 ) ) ;
#8942 = VECTOR ( 'NONE', #6899, 1000.000000000000000 ) ;
#8943 = ORIENTED_EDGE ( 'NONE', *, *, #4613, .T. ) ;
#8944 = LINE ( 'NONE', #10230, #1727 ) ;
#8945 = DIRECTION ( 'NONE',  ( 1.216682766712499758E-16, 3.041706916781249394E-17, 1.000000000000000000 ) ) ;
#8946 = DIRECTION ( 'NONE',  ( 0.000000000000000000, 0.000000000000000000, -1.000000000000000000 ) ) ;
#8947 = CARTESIAN_POINT ( 'NONE',  ( 1.791574935211219799, -5.108686440677970175, 6.226029630577610163 ) ) ;
#8948 = VERTEX_POINT ( 'NONE', #17320 ) ;
#8949 = ORIENTED_EDGE ( 'NONE', *, *, #6467, .T. ) ;
#8950 = LINE ( 'NONE', #7653, #9479 ) ;
#8951 = ORIENTED_EDGE ( 'NONE', *, *, #14397, .T. ) ;
#8952 = EDGE_CURVE ( 'NONE', #7208, #3809, #8916, .T. ) ;
#8953 = DIRECTION ( 'NONE',  ( 0.000000000000000000, 6.123233995736769734E-17, -1.000000000000000000 ) ) ;
#8954 = CARTESIAN_POINT ( 'NONE',  ( 2.282375681463800543, -2.425466949207401690, 3.345793611865401473 ) ) ;
#8955 = CARTESIAN_POINT ( 'NONE',  ( 1.875000000000000000, 0.7500000000000000000, 7.700000000000000178 ) ) ;
#8956 = VECTOR ( 'NONE', #8325, 1000.000000000000000 ) ;
#8957 = DIRECTION ( 'NONE',  ( -1.000000000000000000, 2.220446049250309876E-16, 0.000000000000000000 ) ) ;
#8958 = CARTESIAN_POINT ( 'NONE',  ( 1.286937324407710026, -2.010118636378180224, 2.729584305145179801 ) ) ;
#8960 = EDGE_CURVE ( 'NONE', #14738, #8102, #4620, .T. ) ;
#8959 = CARTESIAN_POINT ( 'NONE',  ( -0.009452110982655114943, -5.299807955295455564, 2.050000000000001155 ) ) ;
#8961 = CARTESIAN_POINT ( 'NONE',  ( -2.065623031241579977, -5.033755237495680213, 3.572193642975310279 ) ) ;
#8962 = PLANE ( 'NONE',  #16051 ) ;
#8963 = CARTESIAN_POINT ( 'NONE',  ( 2.231116159141619981, -0.9117282104686620370, 3.951089877392439664 ) ) ;
#8964 = DIRECTION ( 'NONE',  ( 1.000000000000000000, 0.000000000000000000, 0.000000000000000000 ) ) ;
#8965 = VERTEX_POINT ( 'NONE', #7756 ) ;
#8966 = DIRECTION ( 'NONE',  ( 6.123233995736759873E-17, -6.123233995736759873E-17, 1.000000000000000000 ) ) ;
#8967 = ORIENTED_EDGE ( 'NONE', *, *, #15168, .T. ) ;
#8968 = DIRECTION ( 'NONE',  ( 0.5521576303742329328, -0.5521576303742328218, -0.6246950475544241765 ) ) ;
#8969 = DIRECTION ( 'NONE',  ( -1.000000000000000000, 0.000000000000000000, 0.000000000000000000 ) ) ;
#8970 = ORIENTED_EDGE ( 'NONE', *, *, #2371, .F. ) ;
#8971 = CARTESIAN_POINT ( 'NONE',  ( 0.5921572875253799939, 6.450000000000000178, 1.600000000000000089 ) ) ;
#8972 = CARTESIAN_POINT ( 'NONE',  ( 1.074829861819710075, -2.285737219477669946, 2.606322265575589991 ) ) ;
#8973 = LINE ( 'NONE', #7683, #7320 ) ;
#8974 = SURFACE_STYLE_FILL_AREA ( #15943 ) ;
#8975 = CARTESIAN_POINT ( 'NONE',  ( 0.5500000000000000444, 6.450000000000000178, 2.699264068711930253 ) ) ;
#8976 = CARTESIAN_POINT ( 'NONE',  ( -1.710920205120030069, -1.587088570829020107, 6.316012914303580139 ) ) ;
#8977 = CARTESIAN_POINT ( 'NONE',  ( 1.728413393879709936, -4.311818300558750039, 6.297289212178290185 ) ) ;
#8978 = CARTESIAN_POINT ( 'NONE',  ( 1.945780800405119360, -0.9117282104686613708, 4.045142061754263274 ) ) ;
#8979 = CARTESIAN_POINT ( 'NONE',  ( 1.899999999999999911, 10.00000000000000000, 0.5999999999999999778 ) ) ;
#8980 = DIRECTION ( 'NONE',  ( 0.000000000000000000, -1.000000000000000000, 2.220446049250320181E-15 ) ) ;
#8981 = ORIENTED_EDGE ( 'NONE', *, *, #10322, .F. ) ;
#8982 = CARTESIAN_POINT ( 'NONE',  ( -2.050059171113549183, -0.2224576271186441134, 4.809263467226075228 ) ) ;
#8983 = CARTESIAN_POINT ( 'NONE',  ( 0.6150581927482109412, -4.451548030288480895, 6.971662190339319665 ) ) ;
#8984 = ORIENTED_EDGE ( 'NONE', *, *, #1028, .F. ) ;
#8985 = VERTEX_POINT ( 'NONE', #14457 ) ;
#8986 = CARTESIAN_POINT ( 'NONE',  ( 1.149999999999999911, 6.472933199251450276, 6.846017351831609865 ) ) ;
#8987 = ORIENTED_EDGE ( 'NONE', *, *, #16310, .F. ) ;
#8988 = CARTESIAN_POINT ( 'NONE',  ( -2.046174187462379557, -4.478677194936738992, 5.862719605944011647 ) ) ;
#8989 = CARTESIAN_POINT ( 'NONE',  ( -0.7322514394120432923, -5.586652542372875452, 2.149183891723918993 ) ) ;
#8990 = PLANE ( 'NONE',  #17945 ) ;
#8991 = EDGE_CURVE ( 'NONE', #14727, #8163, #4530, .T. ) ;
#8992 = CARTESIAN_POINT ( 'NONE',  ( -2.616666666666669805, 1.330536610280860259E-16, 4.000000000000000000 ) ) ;
#8993 = ORIENTED_EDGE ( 'NONE', *, *, #8445, .T. ) ;
#8994 = LINE ( 'NONE', #13089, #5850 ) ;
#8995 = CARTESIAN_POINT ( 'NONE',  ( -0.9588981328681495109, -3.613169651910099756, 2.884671871696449230 ) ) ;
#8996 = CARTESIAN_POINT ( 'NONE',  ( -2.650076489488250697, -0.5224576271186435195, 4.841243018609314497 ) ) ;
#8997 = ORIENTED_EDGE ( 'NONE', *, *, #13676, .T. ) ;
#8998 = ORIENTED_EDGE ( 'NONE', *, *, #11534, .F. ) ;
#8999 = DIRECTION ( 'NONE',  ( 0.000000000000000000, 0.000000000000000000, 1.000000000000000000 ) ) ;
#9000 = EDGE_CURVE ( 'NONE', #5973, #7773, #8713, .T. ) ;
#9001 = DIRECTION ( 'NONE',  ( 2.220446049250309876E-16, 0.000000000000000000, -1.000000000000000000 ) ) ;
#9002 = EDGE_CURVE ( 'NONE', #9183, #2304, #1749, .T. ) ;
#9003 = CARTESIAN_POINT ( 'NONE',  ( 2.653886076156968699, -4.125511994252439862, 4.698454755023375284 ) ) ;
#9004 = ORIENTED_EDGE ( 'NONE', *, *, #11474, .F. ) ;
#9005 = EDGE_CURVE ( 'NONE', #2948, #959, #10023, .T. ) ;
#9006 = CARTESIAN_POINT ( 'NONE',  ( 0.4201920264139500372, -3.477280798540340001, 2.384360920086630031 ) ) ;
#9007 = ADVANCED_FACE ( 'NONE', ( #11575 ), #11403, .T. ) ;
#9008 = CARTESIAN_POINT ( 'NONE',  ( 1.750000000000000000, 0.5999999999999999778, 7.550000000000000711 ) ) ;
#9009 = VECTOR ( 'NONE', #6240, 1000.000000000000000 ) ;
#9010 = CARTESIAN_POINT ( 'NONE',  ( 1.385380178477290558, -3.617010528270069525, 3.184868453331423765 ) ) ;
#9011 = CARTESIAN_POINT ( 'NONE',  ( 1.399999999999999911, 0.5999999999999999778, 3.299999999999999822 ) ) ;
#9012 = CARTESIAN_POINT ( 'NONE',  ( 0.5972539422562040956, -1.008722239981790558, 6.664227474374466276 ) ) ;
#9013 = ORIENTED_EDGE ( 'NONE', *, *, #5510, .T. ) ;
#9014 = DIRECTION ( 'NONE',  ( -2.467162276944790449E-16, 0.000000000000000000, -1.000000000000000000 ) ) ;
#9015 = AXIS2_PLACEMENT_3D ( 'NONE', #10021, #11317, #14077 ) ;
#9016 = CARTESIAN_POINT ( 'NONE',  ( 1.440522616026430391, -0.7952867690272208412, 3.241384813161591438 ) ) ;
#9017 = CARTESIAN_POINT ( 'NONE',  ( 2.652408070456659051, -0.6826862039457533005, 4.611427313555195084 ) ) ;
#9018 = EDGE_LOOP ( 'NONE', ( #1044, #17607, #13317, #11043 ) ) ;
#9019 = CARTESIAN_POINT ( 'NONE',  ( 1.869848057046569867, -4.288530012270459935, 6.129130480762009725 ) ) ;
#9020 = DIRECTION ( 'NONE',  ( 1.000000000000000000, -2.220446049250309876E-16, -6.123233995736759873E-17 ) ) ;
#9021 = CARTESIAN_POINT ( 'NONE',  ( -1.875000000000000000, 11.25000000000000000, 8.300000000000000711 ) ) ;
#9022 = CARTESIAN_POINT ( 'NONE',  ( -2.318251751302029984, -5.233262711864409056, 4.294764266798999586 ) ) ;
#9023 = ORIENTED_EDGE ( 'NONE', *, *, #2682, .F. ) ;
#9024 = ORIENTED_EDGE ( 'NONE', *, *, #17656, .F. ) ;
#9025 = LINE ( 'NONE', #6173, #1510 ) ;
#9026 = CARTESIAN_POINT ( 'NONE',  ( -1.899999999999999911, 7.299999999999999822, 0.6099999999999999867 ) ) ;
#9027 = LINE ( 'NONE', #9123, #7595 ) ;
#9028 = EDGE_CURVE ( 'NONE', #7970, #5991, #11669, .T. ) ;
#9029 = ORIENTED_EDGE ( 'NONE', *, *, #10055, .F. ) ;
#9030 = CARTESIAN_POINT ( 'NONE',  ( 0.8642983280852605255, -2.867944426684881254, 7.209203477813407979 ) ) ;
#9031 = VECTOR ( 'NONE', #2870, 1000.000000000000000 ) ;
#9032 = DIRECTION ( 'NONE',  ( 1.059690869644410208E-14, 1.000000000000000000, -1.041146930477340028E-32 ) ) ;
#9033 = LINE ( 'NONE', #444, #7872 ) ;
#9034 = CARTESIAN_POINT ( 'NONE',  ( -1.764807890102220167, -3.221109627369169726, 3.143016121304770039 ) ) ;
#9035 = CARTESIAN_POINT ( 'NONE',  ( 0.9788656693287738353, -5.320452325212859712, 2.556357798777459944 ) ) ;
#9036 = CARTESIAN_POINT ( 'NONE',  ( 0.5606293434988925961, -1.330917399657850497, 7.293994686233932434 ) ) ;
#9037 = CARTESIAN_POINT ( 'NONE',  ( 1.659340743383524552, -5.037500632107527743, 3.040659256616468742 ) ) ;
#9038 = CARTESIAN_POINT ( 'NONE',  ( -0.06264882350515391107, -0.4512711864406790396, 7.052569299041220319 ) ) ;
#9039 = DIRECTION ( 'NONE',  ( 1.000000000000000000, 0.000000000000000000, 0.000000000000000000 ) ) ;
#9040 = CARTESIAN_POINT ( 'NONE',  ( 2.578017356471871135, -5.386440677966105817, 5.329826563567761077 ) ) ;
#9041 = ORIENTED_EDGE ( 'NONE', *, *, #14794, .F. ) ;
#9042 = AXIS2_PLACEMENT_3D ( 'NONE', #1619, #17318, #2922 ) ;
#9043 = EDGE_CURVE ( 'NONE', #11376, #6378, #13064, .T. ) ;
#9044 = CARTESIAN_POINT ( 'NONE',  ( -0.9000000000000000222, -10.00000000000000000, 3.799999999999999822 ) ) ;
#9045 = EDGE_CURVE ( 'NONE', #16779, #7436, #13401, .T. ) ;
#9046 = VERTEX_POINT ( 'NONE', #8891 ) ;
#9047 = DIRECTION ( 'NONE',  ( -3.700743415417190112E-16, -1.000000000000000000, 0.000000000000000000 ) ) ;
#9048 = DIRECTION ( 'NONE',  ( -4.157615153618229646E-15, 1.000000000000000000, 1.972152263052530214E-30 ) ) ;
#9049 = EDGE_CURVE ( 'NONE', #7321, #11273, #14192, .T. ) ;
#9050 = VECTOR ( 'NONE', #12588, 1000.000000000000000 ) ;
#9051 = CARTESIAN_POINT ( 'NONE',  ( 2.169623098572349917, -2.658349832090280529, 5.611855963200990338 ) ) ;
#9052 = CARTESIAN_POINT ( 'NONE',  ( -2.500000000000000000, 0.4000000000000000222, 4.000000000000000000 ) ) ;
#9053 = DIRECTION ( 'NONE',  ( 0.000000000000000000, 4.440892098500630106E-16, -1.000000000000000000 ) ) ;
#9054 = LINE ( 'NONE', #10449, #14143 ) ;
#9055 = AXIS2_PLACEMENT_3D ( 'NONE', #12758, #8319, #2761 ) ;
#9056 = CARTESIAN_POINT ( 'NONE',  ( 2.151546283159470274, -0.8884399221803740421, 3.746273477677459773 ) ) ;
#9057 = VECTOR ( 'NONE', #11221, 1000.000000000000000 ) ;
#9058 = CARTESIAN_POINT ( 'NONE',  ( -0.4735094604798580353, -4.567989471729919870, 7.005327412390699671 ) ) ;
#9059 = CARTESIAN_POINT ( 'NONE',  ( -1.785776242921159884, -4.478677194936736328, 5.712869711683835838 ) ) ;
#9060 = CARTESIAN_POINT ( 'NONE',  ( 1.899999999999999911, 11.25000000000000000, 7.649999999999999467 ) ) ;
#9061 = AXIS2_PLACEMENT_3D ( 'NONE', #9510, #15167, #9595 ) ;
#9062 = PLANE ( 'NONE',  #5605 ) ;
#9063 = ORIENTED_EDGE ( 'NONE', *, *, #16035, .F. ) ;
#9064 = LINE ( 'NONE', #5965, #7629 ) ;
#9065 = CARTESIAN_POINT ( 'NONE',  ( 2.012177589105479392, -0.08453389830508521718, 5.107213040360584877 ) ) ;
#9066 = CARTESIAN_POINT ( 'NONE',  ( -0.2620510901103649815, -3.706322805063249959, 2.361180871966390260 ) ) ;
#9067 = ORIENTED_EDGE ( 'NONE', *, *, #2367, .F. ) ;
#9068 = ORIENTED_EDGE ( 'NONE', *, *, #11229, .T. ) ;
#9069 = DIRECTION ( 'NONE',  ( 0.000000000000000000, 0.000000000000000000, -1.000000000000000000 ) ) ;
#9070 = CIRCLE ( 'NONE', #3184, 0.2000000000000000944 ) ;
#9071 = ORIENTED_EDGE ( 'NONE', *, *, #4503, .T. ) ;
#9072 = VECTOR ( 'NONE', #16911, 1000.000000000000000 ) ;
#9073 = CARTESIAN_POINT ( 'NONE',  ( 0.6628679656440349399, 6.450000000000000178, 1.670710678118660031 ) ) ;
#9074 = CARTESIAN_POINT ( 'NONE',  ( 0.07064654565475687875, -5.148728813559319661, 7.352897294663512717 ) ) ;
#9075 = CARTESIAN_POINT ( 'NONE',  ( 0.3042893218813439438, 6.450000000000000178, 2.170710678118660031 ) ) ;
#9076 = CARTESIAN_POINT ( 'NONE',  ( 2.088297318559229954, -0.3978813559322040283, 5.785136623276629919 ) ) ;
#9077 = AXIS2_PLACEMENT_3D ( 'NONE', #11313, #16865, #18222 ) ;
#9078 = ORIENTED_EDGE ( 'NONE', *, *, #11740, .F. ) ;
#9079 = VECTOR ( 'NONE', #649, 1000.000000000000000 ) ;
#9080 = DIRECTION ( 'NONE',  ( -1.000000000000000000, 0.000000000000000000, 0.000000000000000000 ) ) ;
#9081 = CARTESIAN_POINT ( 'NONE',  ( 2.043688444617268729, -4.102223705964154199, 4.504451070148833836 ) ) ;
#9082 = CARTESIAN_POINT ( 'NONE',  ( 0.2469343877495150108, -0.004449152542373164231, 2.057675570509529539 ) ) ;
#9083 = ORIENTED_EDGE ( 'NONE', *, *, #12109, .F. ) ;
#9084 = ORIENTED_EDGE ( 'NONE', *, *, #1335, .T. ) ;
#9085 = CARTESIAN_POINT ( 'NONE',  ( 2.130266475405040882, -0.04449152542372925012, 3.117337770017949428 ) ) ;
#9086 = EDGE_LOOP ( 'NONE', ( #11886, #767, #10376, #12578 ) ) ;
#9087 = PRESENTATION_LAYER_ASSIGNMENT (  '', '', ( #13540 ) ) ;
#9088 = CARTESIAN_POINT ( 'NONE',  ( -1.378221871957430178, -5.479872881355929870, 6.607619368096279366 ) ) ;
#9089 = DIRECTION ( 'NONE',  ( -0.7071067811865470176, 0.7071067811865480168, 0.000000000000000000 ) ) ;
#9090 = VECTOR ( 'NONE', #16584, 1000.000000000000000 ) ;
#9091 = FACE_OUTER_BOUND ( 'NONE', #8395, .T. ) ;
#9092 = CARTESIAN_POINT ( 'NONE',  ( -1.661700935788390066, -0.2625000000000000111, 3.038299064211610112 ) ) ;
#9093 = CARTESIAN_POINT ( 'NONE',  ( -1.233489123281609645, -4.637854336594775084, 7.049812391606588236 ) ) ;
#9094 = VERTEX_POINT ( 'NONE', #2105 ) ;
#9095 = AXIS2_PLACEMENT_3D ( 'NONE', #9756, #12896, #41 ) ;
#9096 = CARTESIAN_POINT ( 'NONE',  ( -1.611907055891630192, -3.244397915657459830, 2.985210995296889713 ) ) ;
#9097 = DIRECTION ( 'NONE',  ( 0.000000000000000000, 0.000000000000000000, 1.000000000000000000 ) ) ;
#9098 = DIRECTION ( 'NONE',  ( 1.000000000000000000, -1.224646799147350002E-16, 0.000000000000000000 ) ) ;
#9099 = VECTOR ( 'NONE', #5964, 1000.000000000000000 ) ;
#9100 = CARTESIAN_POINT ( 'NONE',  ( 1.353302556710500371, -4.036199717459260761, 6.243850391919140819 ) ) ;
#9101 = VECTOR ( 'NONE', #5173, 1000.000000000000000 ) ;
#9102 = CARTESIAN_POINT ( 'NONE',  ( -0.7500000000000000000, 6.450000000000000178, 3.200000000000000178 ) ) ;
#9103 = DIRECTION ( 'NONE',  ( -1.224646799147350002E-16, -1.000000000000000000, 0.000000000000000000 ) ) ;
#9104 = CARTESIAN_POINT ( 'NONE',  ( -1.058024172752510594, -1.730659176918718956, 2.940600473883360433 ) ) ;
#9105 = VERTEX_POINT ( 'NONE', #2991 ) ;
#9106 = PLANE ( 'NONE',  #4368 ) ;
#9107 = EDGE_CURVE ( 'NONE', #13986, #16755, #4263, .T. ) ;
#9108 = CIRCLE ( 'NONE', #15951, 0.01000000000000002623 ) ;
#9109 = DIRECTION ( 'NONE',  ( -2.220446049250309876E-16, 0.000000000000000000, 1.000000000000000000 ) ) ;
#9110 = CARTESIAN_POINT ( 'NONE',  ( -1.769056124370508964, -1.684082600342149627, 2.721729512470790979 ) ) ;
#9111 = EDGE_CURVE ( 'NONE', #917, #1298, #8545, .T. ) ;
#9112 = ORIENTED_EDGE ( 'NONE', *, *, #17826, .T. ) ;
#9113 = DIRECTION ( 'NONE',  ( -2.168404344971021884E-15, 1.000000000000000000, 0.000000000000000000 ) ) ;
#9114 = CARTESIAN_POINT ( 'NONE',  ( -0.5500000000000000444, 3.050000000000000266, 3.200000000000000178 ) ) ;
#9115 = EDGE_CURVE ( 'NONE', #7642, #1091, #17207, .T. ) ;
#9116 = DIRECTION ( 'NONE',  ( 1.306144734853129823E-16, -1.000000000000000000, -1.306144734853129823E-16 ) ) ;
#9117 = CARTESIAN_POINT ( 'NONE',  ( -0.4360591020458099987, -5.291101694915250064, 2.387347919655840034 ) ) ;
#9118 = ORIENTED_EDGE ( 'NONE', *, *, #13793, .T. ) ;
#9119 = EDGE_LOOP ( 'NONE', ( #14941, #11784, #15193, #9634 ) ) ;
#9120 = LINE ( 'NONE', #10157, #5043 ) ;
#9121 = LINE ( 'NONE', #10614, #10878 ) ;
#9122 = CIRCLE ( 'NONE', #1162, 0.2750000000000000222 ) ;
#9123 = CARTESIAN_POINT ( 'NONE',  ( 0.5500000000000000444, 7.799999999999999822, 3.600000000000000089 ) ) ;
#9124 = ORIENTED_EDGE ( 'NONE', *, *, #13267, .T. ) ;
#9125 = CARTESIAN_POINT ( 'NONE',  ( -1.213493134184840727, -3.314262780522333696, 2.339799138571439396 ) ) ;
#9126 = FACE_OUTER_BOUND ( 'NONE', #5014, .T. ) ;
#9127 = CARTESIAN_POINT ( 'NONE',  ( -2.603140590302631008, -1.726818300558751851, 5.216500493824310247 ) ) ;
#9128 = CARTESIAN_POINT ( 'NONE',  ( -1.899999999999999911, 2.000000000000000000, 1.600000000000000089 ) ) ;
#9129 = CARTESIAN_POINT ( 'NONE',  ( 1.899999999999999911, 2.799999999999999822, 1.600000000000000089 ) ) ;
#9130 = CARTESIAN_POINT ( 'NONE',  ( 2.316639661709690046, -3.780028546288089597, 4.285359956977719875 ) ) ;
#9131 = CARTESIAN_POINT ( 'NONE',  ( 2.500000000000000000, 7.299999999999999822, 1.600000000000000089 ) ) ;
#9132 = EDGE_CURVE ( 'NONE', #8588, #6816, #7423, .T. ) ;
#9134 = ORIENTED_EDGE ( 'NONE', *, *, #1354, .T. ) ;
#9133 = CARTESIAN_POINT ( 'NONE',  ( 2.531332855772549184, -2.635061543801990869, 5.497162258444460825 ) ) ;
#9135 = AXIS2_PLACEMENT_3D ( 'NONE', #18154, #6983, #2644 ) ;
#9136 = DIRECTION ( 'NONE',  ( -1.000000000000000000, 0.000000000000000000, 0.000000000000000000 ) ) ;
#9137 = EDGE_CURVE ( 'NONE', #7321, #5031, #14276, .T. ) ;
#9138 = FACE_OUTER_BOUND ( 'NONE', #11639, .T. ) ;
#9139 = CARTESIAN_POINT ( 'NONE',  ( 2.241103642439659443E-15, 9.099999999999999645, 7.700000000000000178 ) ) ;
#9140 = EDGE_CURVE ( 'NONE', #8561, #2147, #201, .T. ) ;
#9141 = CARTESIAN_POINT ( 'NONE',  ( 2.145694642186089851, -1.098034516774969882, 5.666819626392539888 ) ) ;
#9142 = DIRECTION ( 'NONE',  ( 1.224510688924809779E-16, -1.000000000000000000, -6.530723674265629391E-17 ) ) ;
#9143 = CARTESIAN_POINT ( 'NONE',  ( -1.750316316486840051, -5.559957627118639500, 3.126818518378589928 ) ) ;
#9144 = VERTEX_POINT ( 'NONE', #384 ) ;
#9145 = FACE_OUTER_BOUND ( 'NONE', #6583, .T. ) ;
#9146 = EDGE_LOOP ( 'NONE', ( #1232, #7601, #2578, #14471, #5024, #15443, #17172, #10844 ) ) ;
#9147 = DIRECTION ( 'NONE',  ( 0.000000000000000000, 0.000000000000000000, 1.000000000000000000 ) ) ;
#9148 = CARTESIAN_POINT ( 'NONE',  ( 1.899999999999999911, 1.734980836410520254E-17, 3.278889744907200310 ) ) ;
#9149 = ORIENTED_EDGE ( 'NONE', *, *, #5414, .F. ) ;
#9150 = VECTOR ( 'NONE', #13961, 1000.000000000000000 ) ;
#9151 = ORIENTED_EDGE ( 'NONE', *, *, #16718, .T. ) ;
#9152 = CARTESIAN_POINT ( 'NONE',  ( -1.816660071039029933, -3.170692174432619748, 6.196159040268240936 ) ) ;
#9153 = CARTESIAN_POINT ( 'NONE',  ( -1.889104232906369862, -5.555508474576269506, 3.296507079072529933 ) ) ;
#9154 = CYLINDRICAL_SURFACE ( 'NONE', #5207, 0.1000000000000000472 ) ;
#9155 = CARTESIAN_POINT ( 'NONE',  ( 2.291237445532070094, -0.9350164987569499209, 4.162434510291790346 ) ) ;
#9156 = CARTESIAN_POINT ( 'NONE',  ( -1.630481553867809907, -3.543304787045240101, 3.002862530617889547 ) ) ;
#9157 = CARTESIAN_POINT ( 'NONE',  ( -1.750352751699820963, -1.913124606865061139, 3.627075451280493468 ) ) ;
#9158 = CARTESIAN_POINT ( 'NONE',  ( 1.042222075699120287, -0.1245762711864410871, 6.468743694056166227 ) ) ;
#9159 = EDGE_CURVE ( 'NONE', #11911, #9265, #10110, .T. ) ;
#9160 = CARTESIAN_POINT ( 'NONE',  ( 0.3743405594629510280, -0.4423728813559330009, 7.023440622744399953 ) ) ;
#9161 = DIRECTION ( 'NONE',  ( -1.000000000000000000, 0.000000000000000000, 6.123233995736769734E-17 ) ) ;
#9162 = VECTOR ( 'NONE', #17449, 1000.000000000000000 ) ;
#9163 = CARTESIAN_POINT ( 'NONE',  ( -1.580445181003969912, -0.5580508474576266753, 3.389704561770339630 ) ) ;
#9164 = LINE ( 'NONE', #11778, #16843 ) ;
#9165 = VERTEX_POINT ( 'NONE', #14357 ) ;
#9166 = CARTESIAN_POINT ( 'NONE',  ( 0.1749999999999999889, 6.799999999999999822, 0.5999999999999999778 ) ) ;
#9167 = CARTESIAN_POINT ( 'NONE',  ( -1.669205944673819886, -3.147403886144329643, 6.359065158982450505 ) ) ;
#9168 = ORIENTED_EDGE ( 'NONE', *, *, #17393, .F. ) ;
#9169 = ORIENTED_EDGE ( 'NONE', *, *, #5774, .T. ) ;
#9170 = CARTESIAN_POINT ( 'NONE',  ( 0.5372984490435490645, 4.250000000000000000, 8.300000000000000711 ) ) ;
#9171 = ORIENTED_EDGE ( 'NONE', *, *, #5876, .F. ) ;
#9172 = CARTESIAN_POINT ( 'NONE',  ( -2.500000000000000000, 3.500000000000000000, 0.6099999999999999867 ) ) ;
#9173 = CARTESIAN_POINT ( 'NONE',  ( 2.286166334984490067, -5.086440677966099777, 5.258525443163859947 ) ) ;
#9174 = PRODUCT_DEFINITION_SHAPE ( 'NONE', 'NONE',  #12313 ) ;
#9175 = EDGE_CURVE ( 'NONE', #5801, #2436, #3219, .T. ) ;
#9176 = VECTOR ( 'NONE', #3018, 1000.000000000000000 ) ;
#9177 = CARTESIAN_POINT ( 'NONE',  ( -2.155845792290839835, -0.5447033898305089217, 3.756158857535780271 ) ) ;
#9178 = VERTEX_POINT ( 'NONE', #16367 ) ;
#9179 = CARTESIAN_POINT ( 'NONE',  ( 2.500000000000000000, 11.15000000000000036, -3.616154994493369454E-16 ) ) ;
#9180 = CARTESIAN_POINT ( 'NONE',  ( 0.5302109551885175742, -3.799475958216412153, 2.716624547488259989 ) ) ;
#9181 = CARTESIAN_POINT ( 'NONE',  ( 1.128670402850170174, -0.1290254237288140371, 7.101865548313628373 ) ) ;
#9182 = EDGE_CURVE ( 'NONE', #15500, #5929, #3867, .T. ) ;
#9183 = VERTEX_POINT ( 'NONE', #13868 ) ;
#9184 = CARTESIAN_POINT ( 'NONE',  ( 1.596341326794969984, -0.3355932203389830337, 2.970780074643809776 ) ) ;
#9185 = CARTESIAN_POINT ( 'NONE',  ( 2.458531667407859889, -0.3934322033898309257, 5.699238225248945966 ) ) ;
#9186 = ORIENTED_EDGE ( 'NONE', *, *, #13771, .T. ) ;
#9187 = CARTESIAN_POINT ( 'NONE',  ( -1.000000000000000000, -5.599999999999999645, 3.673738709727309981 ) ) ;
#9188 = CARTESIAN_POINT ( 'NONE',  ( -2.318251751302029984, -5.533262711864409766, 4.294764266798999586 ) ) ;
#9189 = DIRECTION ( 'NONE',  ( -1.059337802663170094E-14, -1.000000000000000000, 0.000000000000000000 ) ) ;
#9190 = CARTESIAN_POINT ( 'NONE',  ( 2.143090896833110381, -5.395338983050850246, 5.672454929438339732 ) ) ;
#9191 = CARTESIAN_POINT ( 'NONE',  ( 0.2010642693393740188, -3.752899381639833720, 2.053740970237999619 ) ) ;
#9192 = VERTEX_POINT ( 'NONE', #17739 ) ;
#9193 = CARTESIAN_POINT ( 'NONE',  ( -0.8092638295168710361, -4.911779243796849492, 2.486823565593869745 ) ) ;
#9194 = CARTESIAN_POINT ( 'NONE',  ( -2.169623098572329933, -2.941650167909710234, 5.611855963201049846 ) ) ;
#9195 = DIRECTION ( 'NONE',  ( -1.142385477618690076E-14, 1.110223024625153952E-16, -1.000000000000000000 ) ) ;
#9196 = DIRECTION ( 'NONE',  ( 1.306144734853129823E-16, -1.000000000000000000, -1.306144734853129823E-16 ) ) ;
#9197 = CARTESIAN_POINT ( 'NONE',  ( 0.5133516189064986079, -4.152641158900696183, 6.687805814961351736 ) ) ;
#9198 = DIRECTION ( 'NONE',  ( 1.000000000000000000, 0.000000000000000000, 0.000000000000000000 ) ) ;
#9199 = DIRECTION ( 'NONE',  ( 0.000000000000000000, 0.000000000000000000, 1.000000000000000000 ) ) ;
#9200 = CARTESIAN_POINT ( 'NONE',  ( 2.029711248330070994, -2.219713230972778728, 4.391497016172514201 ) ) ;
#9201 = VERTEX_POINT ( 'NONE', #2404 ) ;
#9202 = CARTESIAN_POINT ( 'NONE',  ( -1.199999999999880052, 11.40000000000000036, -2.399999999999999911 ) ) ;
#9203 = CARTESIAN_POINT ( 'NONE',  ( 1.097896950867359500, -0.7068739681193977331, 2.280088753565270743 ) ) ;
#9204 = CARTESIAN_POINT ( 'NONE',  ( 0.04661003995938393929, -1.870388906648449812, 2.046522810126899294 ) ) ;
#9205 = VERTEX_POINT ( 'NONE', #12391 ) ;
#9206 = CARTESIAN_POINT ( 'NONE',  ( 1.899999999999999911, 10.00000000000000000, 1.600000000000000089 ) ) ;
#9207 = DIRECTION ( 'NONE',  ( 0.000000000000000000, 0.000000000000000000, -1.000000000000000000 ) ) ;
#9208 = FACE_OUTER_BOUND ( 'NONE', #5544, .T. ) ;
#9209 = ADVANCED_FACE ( 'NONE', ( #13768 ), #17822, .F. ) ;
#9210 = CARTESIAN_POINT ( 'NONE',  ( 2.000624272291700034, -5.064194915254235596, 4.239366054775996595 ) ) ;
#9211 = ORIENTED_EDGE ( 'NONE', *, *, #8237, .F. ) ;
#9212 = ORIENTED_EDGE ( 'NONE', *, *, #9697, .F. ) ;
#9213 = DIRECTION ( 'NONE',  ( 1.000000000000000000, 0.000000000000000000, 2.400482215405740060E-16 ) ) ;
#9214 = CARTESIAN_POINT ( 'NONE',  ( 2.500000000000000000, 9.199999999999999289, 0.5999999999999999778 ) ) ;
#9215 = CARTESIAN_POINT ( 'NONE',  ( 2.500000000000000000, 2.799999999999999822, 1.600000000000000089 ) ) ;
#9216 = EDGE_LOOP ( 'NONE', ( #1037, #8878, #3379, #4276 ) ) ;
#9217 = CARTESIAN_POINT ( 'NONE',  ( -0.5137283630188880235, -5.462076271186444565, 6.687652957477222770 ) ) ;
#9218 = CARTESIAN_POINT ( 'NONE',  ( 2.589141052314449354, -2.312866384125929820, 5.282633936723466483 ) ) ;
#9219 = DIRECTION ( 'NONE',  ( 0.000000000000000000, 0.000000000000000000, 1.000000000000000000 ) ) ;
#9220 = CARTESIAN_POINT ( 'NONE',  ( 2.567863625471588751, -2.495331814072259569, 4.029783546918046078 ) ) ;
#9221 = AXIS2_PLACEMENT_3D ( 'NONE', #12498, #8515, #13889 ) ;
#9222 = FACE_OUTER_BOUND ( 'NONE', #11176, .T. ) ;
#9223 = LINE ( 'NONE', #6261, #1975 ) ;
#9224 = ADVANCED_FACE ( 'NONE', ( #8051 ), #18010, .T. ) ;
#9225 = CARTESIAN_POINT ( 'NONE',  ( -0.2365712905368979879, -3.407415933675480346, 2.358466376073659720 ) ) ;
#9226 = CARTESIAN_POINT ( 'NONE',  ( 1.315859850362970151, -5.328211948015590060, 2.737664967889629875 ) ) ;
#9227 = LINE ( 'NONE', #12295, #5302 ) ;
#9228 = VECTOR ( 'NONE', #3959, 1000.000000000000000 ) ;
#9230 = ORIENTED_EDGE ( 'NONE', *, *, #14906, .F. ) ;
#9229 = CARTESIAN_POINT ( 'NONE',  ( 2.494165244384159763, -2.472043525783979678, 3.793218093085234166 ) ) ;
#9231 = DIRECTION ( 'NONE',  ( -1.665334536937729880E-16, 0.000000000000000000, -1.000000000000000000 ) ) ;
#9232 = CARTESIAN_POINT ( 'NONE',  ( 0.6493550500446280127, -0.3133474576271190193, 2.437955526623099889 ) ) ;
#9233 = CARTESIAN_POINT ( 'NONE',  ( 0.6673090596498160165, -2.239160642901090181, 2.443133963569570355 ) ) ;
#9234 = CARTESIAN_POINT ( 'NONE',  ( -1.791574935211209807, -0.4913135593220339659, 6.226029630577610163 ) ) ;
#9235 = DIRECTION ( 'NONE',  ( -1.000000000000000000, 0.000000000000000000, 0.000000000000000000 ) ) ;
#9236 = CARTESIAN_POINT ( 'NONE',  ( 1.932035991685901122, -5.338983050847455836, 2.884370051397200818 ) ) ;
#9237 = VERTEX_POINT ( 'NONE', #9429 ) ;
#9238 = LINE ( 'NONE', #16287, #12836 ) ;
#9239 = VERTEX_POINT ( 'NONE', #7847 ) ;
#9240 = DIRECTION ( 'NONE',  ( 0.000000000000000000, -1.000000000000000000, -8.881784197001250351E-16 ) ) ;
#9241 = LINE ( 'NONE', #1853, #7946 ) ;
#9242 = EDGE_CURVE ( 'NONE', #10396, #11911, #9227, .T. ) ;
#9243 = ORIENTED_EDGE ( 'NONE', *, *, #2868, .F. ) ;
#9244 = VECTOR ( 'NONE', #15988, 1000.000000000000000 ) ;
#9245 = ADVANCED_FACE ( 'NONE', ( #5067 ), #6454, .T. ) ;
#9246 = ORIENTED_EDGE ( 'NONE', *, *, #2452, .F. ) ;
#9247 = CARTESIAN_POINT ( 'NONE',  ( -1.948278411993560111, -3.193980462720909852, 6.020210936496040333 ) ) ;
#9248 = EDGE_CURVE ( 'NONE', #959, #16239, #16276, .T. ) ;
#9249 = DIRECTION ( 'NONE',  ( -0.000000000000000000, 1.000000000000000000, 0.000000000000000000 ) ) ;
#9250 = CARTESIAN_POINT ( 'NONE',  ( -0.6493550500446439999, -5.586652542372879005, 2.437955526623099889 ) ) ;
#9251 = EDGE_CURVE ( 'NONE', #4807, #16560, #2567, .T. ) ;
#9252 = DIRECTION ( 'NONE',  ( 1.000000000000000000, 0.000000000000000000, 0.000000000000000000 ) ) ;
#9253 = EDGE_CURVE ( 'NONE', #10029, #851, #6638, .T. ) ;
#9254 = CARTESIAN_POINT ( 'NONE',  ( -1.741913176380149864, -1.959701183441629802, 3.117443785062560035 ) ) ;
#9255 = EDGE_CURVE ( 'NONE', #16609, #5167, #14890, .T. ) ;
#9256 = CARTESIAN_POINT ( 'NONE',  ( 0.1824815401350060040, -4.498124606865050445, 7.046368721022729709 ) ) ;
#9257 = CARTESIAN_POINT ( 'NONE',  ( -0.7368491673940088527, -2.076142624883081211, 2.783765372628170809 ) ) ;
#9258 = FACE_OUTER_BOUND ( 'NONE', #10378, .T. ) ;
#9259 = CARTESIAN_POINT ( 'NONE',  ( -1.661700935788390066, -0.5625000000000000000, 3.038299064211610112 ) ) ;
#9260 = ORIENTED_EDGE ( 'NONE', *, *, #3574, .T. ) ;
#9261 = CARTESIAN_POINT ( 'NONE',  ( 1.656536077435048604, -0.4969333835596383420, 3.061489489342141823 ) ) ;
#9262 = DIRECTION ( 'NONE',  ( 0.000000000000000000, 0.000000000000000000, 1.000000000000000000 ) ) ;
#9263 = CARTESIAN_POINT ( 'NONE',  ( 1.397172971746949877, -3.892629111369559691, 2.806153814454899642 ) ) ;
#9264 = ORIENTED_EDGE ( 'NONE', *, *, #12422, .T. ) ;
#9265 = VERTEX_POINT ( 'NONE', #10719 ) ;
#9266 = CARTESIAN_POINT ( 'NONE',  ( -1.889999999999999902, 7.299999999999999822, 0.5999999999999999778 ) ) ;
#9267 = ORIENTED_EDGE ( 'NONE', *, *, #3469, .F. ) ;
#9268 = CARTESIAN_POINT ( 'NONE',  ( -1.803891155489809606, -4.781424942684489920, 3.188470185434129966 ) ) ;
#9269 = APPLICATION_PROTOCOL_DEFINITION ( 'draft international standard', 'automotive_design', 1998, #830 ) ;
#9270 = CARTESIAN_POINT ( 'NONE',  ( 1.713314936023349944, -5.038983050847460454, 3.089913064446569546 ) ) ;
#9271 = EDGE_CURVE ( 'NONE', #8938, #6834, #3671, .T. ) ;
#9272 = CARTESIAN_POINT ( 'NONE',  ( -1.850000000000000089, 11.25000000000000000, 7.700000000000000178 ) ) ;
#9273 = ORIENTED_EDGE ( 'NONE', *, *, #7864, .F. ) ;
#9274 = FACE_OUTER_BOUND ( 'NONE', #1216, .T. ) ;
#9275 = CARTESIAN_POINT ( 'NONE',  ( -0.4194839839382230595, -3.683034516774964295, 2.690289814463939777 ) ) ;
#9276 = CARTESIAN_POINT ( 'NONE',  ( 2.130266475405040882, -0.04449152542372925012, 3.117337770017949428 ) ) ;
#9277 = ORIENTED_EDGE ( 'NONE', *, *, #17389, .T. ) ;
#9278 = CARTESIAN_POINT ( 'NONE',  ( 1.057242234132090175, -0.3222457627118650025, 2.597442975781520058 ) ) ;
#9279 = VERTEX_POINT ( 'NONE', #9319 ) ;
#9280 = CARTESIAN_POINT ( 'NONE',  ( 1.596341326794969984, -0.03559322033898330156, 2.970780074643809776 ) ) ;
#9281 = ORIENTED_EDGE ( 'NONE', *, *, #9591, .F. ) ;
#9282 = CARTESIAN_POINT ( 'NONE',  ( -2.088297318559229954, -5.502118644067800268, 5.785136623276639689 ) ) ;
#9283 = CARTESIAN_POINT ( 'NONE',  ( 0.6864473529425536569, -1.008722239981789892, 6.951118770549889803 ) ) ;
#9284 = CARTESIAN_POINT ( 'NONE',  ( -1.661700935788390066, -0.5625000000000000000, 3.038299064211610112 ) ) ;
#9285 = CARTESIAN_POINT ( 'NONE',  ( 2.524473153133520054, -0.6128213390808875394, 3.881373716577345867 ) ) ;
#9286 = EDGE_CURVE ( 'NONE', #10172, #5295, #12206, .T. ) ;
#9287 = ORIENTED_EDGE ( 'NONE', *, *, #5182, .T. ) ;
#9288 = DIRECTION ( 'NONE',  ( 0.000000000000000000, 0.000000000000000000, 1.000000000000000000 ) ) ;
#9289 = CARTESIAN_POINT ( 'NONE',  ( 2.028464043723889887, -0.7292627805223297344, 5.016599851465070259 ) ) ;
#9290 = CARTESIAN_POINT ( 'NONE',  ( -1.447263454062130528, -4.661142624883069630, 6.924531903016462486 ) ) ;
#9291 = DIRECTION ( 'NONE',  ( -4.898587196589410857E-16, -1.000000000000000000, 3.081487911019575175E-31 ) ) ;
#9292 = LINE ( 'NONE', #5133, #9684 ) ;
#9293 = CARTESIAN_POINT ( 'NONE',  ( 1.889999999999999902, 7.900000000000000355, 3.000000000000000000 ) ) ;
#9294 = CARTESIAN_POINT ( 'NONE',  ( 1.279347147864559275, -2.033406924666469884, 3.094331068408280760 ) ) ;
#9295 = VERTEX_POINT ( 'NONE', #9604 ) ;
#9296 = DIRECTION ( 'NONE',  ( 1.000000000000000000, 3.700743415417199972E-16, 0.000000000000000000 ) ) ;
#9297 = CARTESIAN_POINT ( 'NONE',  ( -1.899999999999999911, 0.5999999999999999778, 1.600000000000000089 ) ) ;
#9298 = CARTESIAN_POINT ( 'NONE',  ( 0.2554393686801398333, -0.6247245358507580448, 2.048880876762550596 ) ) ;
#9299 = CARTESIAN_POINT ( 'NONE',  ( 0.1110902655589990351, -2.638902420161969520, 7.351560417169478612 ) ) ;
#9300 = ORIENTED_EDGE ( 'NONE', *, *, #14858, .F. ) ;
#9301 = LINE ( 'NONE', #10703, #14685 ) ;
#9302 = CARTESIAN_POINT ( 'NONE',  ( 2.231116159141619981, -0.9117282104686620370, 3.951089877392439664 ) ) ;
#9303 = CARTESIAN_POINT ( 'NONE',  ( 0.5500000000000000444, 6.450000000000000178, 1.600000000000000089 ) ) ;
#9304 = CARTESIAN_POINT ( 'NONE',  ( -2.011500846714319835, -5.251059322033900578, 3.478373409938470218 ) ) ;
#9305 = ORIENTED_EDGE ( 'NONE', *, *, #1449, .F. ) ;
#9306 = ORIENTED_EDGE ( 'NONE', *, *, #1822, .F. ) ;
#9307 = DIRECTION ( 'NONE',  ( 0.000000000000000000, 3.965082230804129973E-17, -1.000000000000000000 ) ) ;
#9308 = FACE_OUTER_BOUND ( 'NONE', #6352, .T. ) ;
#9309 = CARTESIAN_POINT ( 'NONE',  ( -1.800000000000000044, 7.799999999999999822, 1.600000000000000089 ) ) ;
#9310 = ORIENTED_EDGE ( 'NONE', *, *, #14259, .T. ) ;
#9311 = CARTESIAN_POINT ( 'NONE',  ( 2.332582362116870200, -5.368644067796609853, 4.387643303570810005 ) ) ;
#9312 = CARTESIAN_POINT ( 'NONE',  ( 1.963178672446078687, -3.640298816558361406, 2.914210764660420061 ) ) ;
#9313 = DIRECTION ( 'NONE',  ( -1.000000000000000000, 0.000000000000000000, 0.000000000000000000 ) ) ;
#9314 = CARTESIAN_POINT ( 'NONE',  ( 1.000000000000000000, 6.400000000000000355, 7.700000000000000178 ) ) ;
#9315 = DIRECTION ( 'NONE',  ( -3.416070845000479880E-16, -1.000000000000000000, -5.978123978750840407E-16 ) ) ;
#9316 = CARTESIAN_POINT ( 'NONE',  ( 1.741913176380120110, -3.640298816558360073, 3.117443785062520067 ) ) ;
#9317 = AXIS2_PLACEMENT_3D ( 'NONE', #14014, #17286, #9660 ) ;
#9318 = DIRECTION ( 'NONE',  ( 0.000000000000000000, -1.000000000000000000, 0.000000000000000000 ) ) ;
#9319 = CARTESIAN_POINT ( 'NONE',  ( -0.1749999999999999889, 2.700000000000000178, 1.600000000000000089 ) ) ;
#9321 = VERTEX_POINT ( 'NONE', #13600 ) ;
#9320 = CARTESIAN_POINT ( 'NONE',  ( -1.597383073937548970, -2.006277760018210898, 2.580688553303291943 ) ) ;
#9322 = FACE_OUTER_BOUND ( 'NONE', #3468, .T. ) ;
#9323 = DIRECTION ( 'NONE',  ( -6.162975822039146519E-33, -0.2588190451025180749, 0.9659258262890690894 ) ) ;
#9324 = CARTESIAN_POINT ( 'NONE',  ( -0.5902886515192680150, -1.447358841099289917, 6.978224088050050788 ) ) ;
#9325 = DIRECTION ( 'NONE',  ( 7.300096600275009393E-16, -1.215710299141969852E-31, 1.000000000000000000 ) ) ;
#9326 = CARTESIAN_POINT ( 'NONE',  ( 1.670747152266691016, -0.4963810343603142217, 3.047345280935851441 ) ) ;
#9327 = CARTESIAN_POINT ( 'NONE',  ( -1.549742865090599997, -5.484322033898309634, 6.471102547561460305 ) ) ;
#9328 = VERTEX_POINT ( 'NONE', #6553 ) ;
#9329 =( NAMED_UNIT ( * ) PLANE_ANGLE_UNIT ( ) SI_UNIT ( $, .RADIAN. ) );
#9330 = ORIENTED_EDGE ( 'NONE', *, *, #6169, .F. ) ;
#9331 = CARTESIAN_POINT ( 'NONE',  ( 1.641808337277749663, -5.113135593220338393, 6.386111670537620633 ) ) ;
#9332 = FACE_OUTER_BOUND ( 'NONE', #4440, .T. ) ;
#9333 = CARTESIAN_POINT ( 'NONE',  ( -1.899999999999999911, 11.40000000000000036, 6.599999999999999645 ) ) ;
#9334 = VECTOR ( 'NONE', #15826, 1000.000000000000000 ) ;
#9335 = ORIENTED_EDGE ( 'NONE', *, *, #7444, .T. ) ;
#9336 = CARTESIAN_POINT ( 'NONE',  ( 2.075124426334590044, -2.681638120378570189, 5.810227140144509583 ) ) ;
#9337 = DIRECTION ( 'NONE',  ( 1.708035422500239940E-16, -1.000000000000000000, -8.540177112501209562E-17 ) ) ;
#9338 = CARTESIAN_POINT ( 'NONE',  ( 1.925796468768800063, -5.404237288135590234, 6.052706598917719560 ) ) ;
#9339 = DIRECTION ( 'NONE',  ( 0.000000000000000000, 1.000000000000000000, 0.000000000000000000 ) ) ;
#9340 = CARTESIAN_POINT ( 'NONE',  ( 1.167621112247380077, -2.821367850108300157, 6.743381174846749815 ) ) ;
#9341 = PLANE ( 'NONE',  #2843 ) ;
#9342 = CARTESIAN_POINT ( 'NONE',  ( -2.021195349941399044, -1.819971453711898945, 4.339901124684693912 ) ) ;
#9343 = VECTOR ( 'NONE', #422, 1000.000000000000000 ) ;
#9344 = CARTESIAN_POINT ( 'NONE',  ( -0.1749999999999999889, 5.200000000000000178, 1.600000000000000089 ) ) ;
#9345 = CARTESIAN_POINT ( 'NONE',  ( -0.5198535559317755128, -0.5906145504024216120, 2.087183161631441131 ) ) ;
#9346 = ORIENTED_EDGE ( 'NONE', *, *, #15827, .F. ) ;
#9347 = EDGE_CURVE ( 'NONE', #8260, #12172, #10809, .T. ) ;
#9348 = CARTESIAN_POINT ( 'NONE',  ( -2.500000000000000000, 9.199999999999999289, 1.600000000000000089 ) ) ;
#9349 = DIRECTION ( 'NONE',  ( 1.000000000000000000, -7.401486830834380223E-16, 0.000000000000000000 ) ) ;
#9350 = CARTESIAN_POINT ( 'NONE',  ( -0.6914213562373099364, 3.050000000000000266, 2.557842712474620139 ) ) ;
#9351 = VERTEX_POINT ( 'NONE', #16558 ) ;
#9352 = EDGE_CURVE ( 'NONE', #7150, #9659, #14453, .T. ) ;
#9353 = ORIENTED_EDGE ( 'NONE', *, *, #4599, .T. ) ;
#9354 = EDGE_CURVE ( 'NONE', #8456, #11761, #1090, .T. ) ;
#9355 = DIRECTION ( 'NONE',  ( 1.368455531567199917E-48, 1.000000000000000000, 1.233581138472399909E-16 ) ) ;
#9356 = ORIENTED_EDGE ( 'NONE', *, *, #11513, .F. ) ;
#9357 = APPLICATION_PROTOCOL_DEFINITION ( 'draft international standard', 'automotive_design', 1998, #8745 ) ;
#9358 = CARTESIAN_POINT ( 'NONE',  ( -2.088297318559229954, -5.202118644067800446, 5.785136623276639689 ) ) ;
#9359 = CIRCLE ( 'NONE', #1382, 0.9499999999999999556 ) ;
#9360 = CIRCLE ( 'NONE', #12925, 0.5000000000000004441 ) ;
#9361 = DIRECTION ( 'NONE',  ( 8.326672684688679970E-16, 0.000000000000000000, 1.000000000000000000 ) ) ;
#9362 = AXIS2_PLACEMENT_3D ( 'NONE', #17751, #5082, #9047 ) ;
#9363 = ORIENTED_EDGE ( 'NONE', *, *, #4173, .T. ) ;
#9364 = CARTESIAN_POINT ( 'NONE',  ( -2.650521604678268694, -4.595118636378185073, 4.833599835830360014 ) ) ;
#9365 = DIRECTION ( 'NONE',  ( -0.000000000000000000, 1.000000000000000000, 0.000000000000000000 ) ) ;
#9366 = CARTESIAN_POINT ( 'NONE',  ( -1.881914957835490121, -1.936412895153350133, 3.286797332666350435 ) ) ;
#9367 = CIRCLE ( 'NONE', #12032, 0.4000000000000001887 ) ;
#9368 = CARTESIAN_POINT ( 'NONE',  ( -2.519547246525518425, -0.2402542372881359412, 3.866491354109200529 ) ) ;
#9369 = EDGE_CURVE ( 'NONE', #15033, #229, #15262, .T. ) ;
#9370 = EDGE_LOOP ( 'NONE', ( #14755, #7676, #14865, #8279 ) ) ;
#9371 = CARTESIAN_POINT ( 'NONE',  ( -1.869504824896970119, -0.5046610169491535514, 5.548311746956866131 ) ) ;
#9372 = ORIENTED_EDGE ( 'NONE', *, *, #12249, .T. ) ;
#9373 = EDGE_CURVE ( 'NONE', #11111, #1650, #17520, .T. ) ;
#9374 = AXIS2_PLACEMENT_3D ( 'NONE', #9102, #13572, #6324 ) ;
#9375 = CARTESIAN_POINT ( 'NONE',  ( 1.428515267734870031, -0.03114406779661050076, 2.829745655876919841 ) ) ;
#9376 = AXIS2_PLACEMENT_3D ( 'NONE', #4554, #7268, #3097 ) ;
#9377 = ORIENTED_EDGE ( 'NONE', *, *, #4307, .T. ) ;
#9378 = VECTOR ( 'NONE', #17649, 1000.000000000000000 ) ;
#9379 = CARTESIAN_POINT ( 'NONE',  ( 1.713314936023349722, -5.038983050847458678, 3.089913064446569546 ) ) ;
#9380 = CARTESIAN_POINT ( 'NONE',  ( -1.149999999999999911, 9.299999999999998934, 7.599999999999999645 ) ) ;
#9381 = DIRECTION ( 'NONE',  ( 0.000000000000000000, -1.000000000000000000, 0.000000000000000000 ) ) ;
#9382 = CARTESIAN_POINT ( 'NONE',  ( 0.5999999999999999778, 0.5999999999999999778, 7.700000000000000178 ) ) ;
#9383 = CARTESIAN_POINT ( 'NONE',  ( -0.5889081234606770021, -5.462076271186440124, 6.978529000034869867 ) ) ;
#9384 = VECTOR ( 'NONE', #8360, 1000.000000000000000 ) ;
#9385 = VECTOR ( 'NONE', #1872, 1000.000000000000000 ) ;
#9386 = AXIS2_PLACEMENT_3D ( 'NONE', #12981, #8811, #13068 ) ;
#9387 = CARTESIAN_POINT ( 'NONE',  ( 1.447263454062181598, -0.9388573751169233539, 6.924531903016430512 ) ) ;
#9388 = VERTEX_POINT ( 'NONE', #4849 ) ;
#9389 = LINE ( 'NONE', #12080, #14947 ) ;
#9390 = EDGE_CURVE ( 'NONE', #17860, #16352, #15944, .T. ) ;
#9391 = CARTESIAN_POINT ( 'NONE',  ( 2.091095264232530226, -3.943046564306110113, 5.779845490516200002 ) ) ;
#9392 = CARTESIAN_POINT ( 'NONE',  ( -1.940935473245981147, -5.095857339597785973, 2.893832807158200016 ) ) ;
#9393 = AXIS2_PLACEMENT_3D ( 'NONE', #9673, #15244, #2545 ) ;
#9394 = CARTESIAN_POINT ( 'NONE',  ( -1.899999999999999911, 4.700000000000000178, 0.6099999999999999867 ) ) ;
#9395 = VECTOR ( 'NONE', #12475, 1000.000000000000000 ) ;
#9396 = CARTESIAN_POINT ( 'NONE',  ( -0.6217226704572171858, -4.292370888630430592, 6.656620240022991908 ) ) ;
#9397 = DIRECTION ( 'NONE',  ( 0.000000000000000000, 0.000000000000000000, 1.000000000000000000 ) ) ;
#9398 = DIRECTION ( 'NONE',  ( 1.306144734853129823E-16, 6.530723674265629391E-17, -1.000000000000000000 ) ) ;
#9399 = CARTESIAN_POINT ( 'NONE',  ( 1.951270856817530319, -2.336154672414218592, 5.338313313320885989 ) ) ;
#9400 = ORIENTED_EDGE ( 'NONE', *, *, #11740, .T. ) ;
#9401 = CARTESIAN_POINT ( 'NONE',  ( 1.899999999999999911, 0.7500000000000000000, 7.649999999999999467 ) ) ;
#9402 = PLANE ( 'NONE',  #17657 ) ;
#9403 = CIRCLE ( 'NONE', #11773, 0.3499999999999999778 ) ;
#9404 = VECTOR ( 'NONE', #18037, 1000.000000000000000 ) ;
#9405 = EDGE_CURVE ( 'NONE', #2627, #15044, #10494, .T. ) ;
#9406 = CARTESIAN_POINT ( 'NONE',  ( 1.118481890237429610, -0.4076464065212261345, 2.289482119763390333 ) ) ;
#9407 = CARTESIAN_POINT ( 'NONE',  ( -2.635341251434490495, -3.011515032774579215, 5.013193520829514860 ) ) ;
#9408 = ORIENTED_EDGE ( 'NONE', *, *, #15171, .T. ) ;
#9409 = DIRECTION ( 'NONE',  ( -1.000000000000000000, -1.708035422500239940E-16, -4.440892098500630106E-16 ) ) ;
#9410 = DIRECTION ( 'NONE',  ( -1.000000000000000000, 0.000000000000000000, 0.000000000000000000 ) ) ;
#9411 = CARTESIAN_POINT ( 'NONE',  ( -3.421358338620380043E-15, -5.299999999999999822, 2.350000000000000089 ) ) ;
#9412 = EDGE_LOOP ( 'NONE', ( #14560, #16412, #10258, #1901 ) ) ;
#9413 = AXIS2_PLACEMENT_3D ( 'NONE', #16611, #9476, #3831 ) ;
#9414 = ORIENTED_EDGE ( 'NONE', *, *, #2350, .F. ) ;
#9415 = DIRECTION ( 'NONE',  ( 1.224646799147350002E-16, -1.000000000000000000, -6.123233995736769734E-17 ) ) ;
#9416 = LINE ( 'NONE', #13299, #2612 ) ;
#9417 = DIRECTION ( 'NONE',  ( -1.000000000000000000, 2.220446049250310320E-15, 0.000000000000000000 ) ) ;
#9418 = ORIENTED_EDGE ( 'NONE', *, *, #16295, .T. ) ;
#9419 = CARTESIAN_POINT ( 'NONE',  ( 1.791574935211219799, -5.408686440677969998, 6.226029630577610163 ) ) ;
#9420 = AXIS2_PLACEMENT_3D ( 'NONE', #16826, #13871, #2847 ) ;
#9421 = AXIS2_PLACEMENT_3D ( 'NONE', #15376, #13707, #2680 ) ;
#9422 = CARTESIAN_POINT ( 'NONE',  ( -0.06913820924137326074, -4.222506023765566496, 7.352985789827153340 ) ) ;
#9423 = CARTESIAN_POINT ( 'NONE',  ( 0.5372984490435490645, 4.599999999999999645, 7.700000000000000178 ) ) ;
#9424 = VECTOR ( 'NONE', #9642, 1000.000000000000000 ) ;
#9425 = FACE_OUTER_BOUND ( 'NONE', #7881, .T. ) ;
#9426 = CARTESIAN_POINT ( 'NONE',  ( 1.586727176531399941, -3.617010528270069969, 2.961885344765599726 ) ) ;
#9427 = DIRECTION ( 'NONE',  ( -4.433365283261159518E-17, 1.000000000000000000, 0.000000000000000000 ) ) ;
#9428 = CIRCLE ( 'NONE', #14144, 0.4166666666666670737 ) ;
#9429 = CARTESIAN_POINT ( 'NONE',  ( -0.5291502622129179434, 0.1000000000000000056, 7.700000000000000178 ) ) ;
#9431 = EDGE_LOOP ( 'NONE', ( #14311, #11969, #16293, #6230, #9858, #11372 ) ) ;
#9430 = CARTESIAN_POINT ( 'NONE',  ( 2.445954350973281510, -2.658349832090279197, 5.729767452368150771 ) ) ;
#9432 = EDGE_CURVE ( 'NONE', #458, #1463, #15893, .T. ) ;
#9433 = LINE ( 'NONE', #628, #3795 ) ;
#9434 = CARTESIAN_POINT ( 'NONE',  ( 1.899999999999999911, 2.000000000000000000, 1.600000000000000089 ) ) ;
#9435 = VECTOR ( 'NONE', #10177, 1000.000000000000000 ) ;
#9436 = CARTESIAN_POINT ( 'NONE',  ( -2.199335452462570117, -1.866548030288480042, 3.862342996790939953 ) ) ;
#9437 = CARTESIAN_POINT ( 'NONE',  ( -0.006659065580996091117, -5.255540550750799511, 2.241023775284449737 ) ) ;
#9438 = CARTESIAN_POINT ( 'NONE',  ( -1.899999999999999911, 0.7500000000000000000, 7.649999999999999467 ) ) ;
#9439 = CARTESIAN_POINT ( 'NONE',  ( -2.116444151961480280, -5.546610169491529518, 3.670839500609359707 ) ) ;
#9440 = ORIENTED_EDGE ( 'NONE', *, *, #17487, .T. ) ;
#9441 = ORIENTED_EDGE ( 'NONE', *, *, #16967, .T. ) ;
#9442 = CARTESIAN_POINT ( 'NONE',  ( -0.5889081234606770021, -5.162076271186438525, 6.978529000034869867 ) ) ;
#9443 = DIRECTION ( 'NONE',  ( 0.000000000000000000, 1.000000000000000000, 1.359631073446889961E-32 ) ) ;
#9444 = CARTESIAN_POINT ( 'NONE',  ( -0.007508403481306110717, -0.5690018372754820364, 2.444053578789350034 ) ) ;
#9445 = EDGE_LOOP ( 'NONE', ( #14036, #5366, #4224, #8330, #12069, #13616 ) ) ;
#9446 = CARTESIAN_POINT ( 'NONE',  ( -2.351999299633229956, -3.333710192450639820, 4.782734406438290620 ) ) ;
#9447 = LINE ( 'NONE', #8150, #10888 ) ;
#9448 = CARTESIAN_POINT ( 'NONE',  ( -0.7983658734557950165, -5.466525423728810118, 6.913847129767330735 ) ) ;
#9449 = VECTOR ( 'NONE', #8898, 1000.000000000000000 ) ;
#9450 = DIRECTION ( 'NONE',  ( -1.000000000000000000, 0.000000000000000000, 0.000000000000000000 ) ) ;
#9451 = CARTESIAN_POINT ( 'NONE',  ( -1.507201387235980183, -3.124115597856050197, 6.507509243627219497 ) ) ;
#9452 = EDGE_CURVE ( 'NONE', #8790, #11991, #14501, .T. ) ;
#9453 = CARTESIAN_POINT ( 'NONE',  ( -1.951437470830620136, -5.057043525783970317, 3.384463041838880137 ) ) ;
#9454 = CARTESIAN_POINT ( 'NONE',  ( 2.025702773739959106, -2.518620102360551893, 4.366188503657621567 ) ) ;
#9455 = LINE ( 'NONE', #3977, #6753 ) ;
#9456 = FACE_OUTER_BOUND ( 'NONE', #5400, .T. ) ;
#9457 = VERTEX_POINT ( 'NONE', #1823 ) ;
#9458 = DIRECTION ( 'NONE',  ( 1.850371707708589879E-16, -1.000000000000000000, 0.000000000000000000 ) ) ;
#9459 = CARTESIAN_POINT ( 'NONE',  ( -1.282210379528740063, -4.661142624883069630, 6.673494927815290190 ) ) ;
#9460 = ORIENTED_EDGE ( 'NONE', *, *, #14789, .T. ) ;
#9461 = ORIENTED_EDGE ( 'NONE', *, *, #15614, .F. ) ;
#9462 = EDGE_LOOP ( 'NONE', ( #11247, #15651, #9246, #854, #17587, #16675, #2837, #14721, #11917, #14918, #17583, #3507, #6883, #12697, #8165, #11216 ) ) ;
#9463 = CARTESIAN_POINT ( 'NONE',  ( -2.331386066015260106, -4.641695212954759953, 4.378465089518192244 ) ) ;
#9464 = CARTESIAN_POINT ( 'NONE',  ( 1.477796163681079911, -5.117584745762710163, 6.531563725478140015 ) ) ;
#9465 = DIRECTION ( 'NONE',  ( -2.220446049250309876E-16, 0.000000000000000000, 1.000000000000000000 ) ) ;
#9466 = CARTESIAN_POINT ( 'NONE',  ( 1.875000000000000000, -2.296212748401290437E-16, 7.700000000000000178 ) ) ;
#9467 = CARTESIAN_POINT ( 'NONE',  ( -0.1824815401349519917, -1.101875393134939873, 7.046368721022739479 ) ) ;
#9468 = DIRECTION ( 'NONE',  ( 0.000000000000000000, -1.000000000000000000, 0.000000000000000000 ) ) ;
#9469 = ADVANCED_FACE ( 'NONE', ( #6062 ), #1900, .F. ) ;
#9470 = AXIS2_PLACEMENT_3D ( 'NONE', #350, #1643, #1907 ) ;
#9471 = CARTESIAN_POINT ( 'NONE',  ( -1.802718065953990978, -5.033755237495684653, 3.717600174934233781 ) ) ;
#9472 = CARTESIAN_POINT ( 'NONE',  ( -2.431060148753501515, -0.2447033898305090438, 3.635668498923334102 ) ) ;
#9473 = ORIENTED_EDGE ( 'NONE', *, *, #14466, .F. ) ;
#9474 = CARTESIAN_POINT ( 'NONE',  ( -1.254903241568450900, -0.1735169491525429541, 7.038391080368498365 ) ) ;
#9475 = ORIENTED_EDGE ( 'NONE', *, *, #15981, .F. ) ;
#9476 = DIRECTION ( 'NONE',  ( 0.000000000000000000, 0.000000000000000000, -1.000000000000000000 ) ) ;
#9477 = FACE_OUTER_BOUND ( 'NONE', #14070, .T. ) ;
#9478 = PLANE ( 'NONE',  #44 ) ;
#9479 = VECTOR ( 'NONE', #354, 1000.000000000000000 ) ;
#9480 =( LENGTH_UNIT ( ) NAMED_UNIT ( * ) SI_UNIT ( .MILLI., .METRE. ) );
#9481 = CARTESIAN_POINT ( 'NONE',  ( -2.253200202764409799, -5.511016949152540256, 5.379408587037509903 ) ) ;
#9482 = CARTESIAN_POINT ( 'NONE',  ( -2.107551805806941125, -1.311469987729540376, 6.312866726931216199 ) ) ;
#9483 = VERTEX_POINT ( 'NONE', #17344 ) ;
#9484 = ADVANCED_FACE ( 'NONE', ( #4676 ), #15991, .T. ) ;
#9485 = DIRECTION ( 'NONE',  ( 0.000000000000000000, -1.000000000000000000, 0.000000000000000000 ) ) ;
#9486 = CARTESIAN_POINT ( 'NONE',  ( -1.936998685628559924, -4.758136654396199816, 3.363294429306559863 ) ) ;
#9487 = ADVANCED_FACE ( 'NONE', ( #2178 ), #3736, .T. ) ;
#9488 = CARTESIAN_POINT ( 'NONE',  ( 2.471388659209138972, -4.218665147405589622, 5.667135868497455320 ) ) ;
#9489 = EDGE_CURVE ( 'NONE', #8884, #9633, #7820, .T. ) ;
#9490 = CARTESIAN_POINT ( 'NONE',  ( -1.289999999999999813, 7.900000000000014566, 0.6000000000000020872 ) ) ;
#9491 = CARTESIAN_POINT ( 'NONE',  ( 1.250000000000000000, 0.5999999999999999778, 6.100000000000000533 ) ) ;
#9492 = EDGE_CURVE ( 'NONE', #2762, #6171, #10033, .T. ) ;
#9493 = CARTESIAN_POINT ( 'NONE',  ( 2.032257487115179728, -1.028169651910100679, 4.991258216523873692 ) ) ;
#9494 = ADVANCED_FACE ( 'NONE', ( #2267 ), #10595, .T. ) ;
#9495 = FACE_BOUND ( 'NONE', #8767, .T. ) ;
#9496 = DIRECTION ( 'NONE',  ( 0.000000000000000000, 0.000000000000000000, 1.000000000000000000 ) ) ;
#9497 = ORIENTED_EDGE ( 'NONE', *, *, #15225, .F. ) ;
#9498 = CYLINDRICAL_SURFACE ( 'NONE', #3919, 1.000000000000000000 ) ;
#9499 = VECTOR ( 'NONE', #10464, 1000.000000000000000 ) ;
#9500 = DIRECTION ( 'NONE',  ( 7.930164461608259947E-17, -1.000000000000000000, 0.000000000000000000 ) ) ;
#9501 = CARTESIAN_POINT ( 'NONE',  ( 1.647941990407678636, -0.3444915254237289615, 3.475676388127089123 ) ) ;
#9502 = DIRECTION ( 'NONE',  ( 0.000000000000000000, -1.000000000000000000, -6.123233995736769734E-17 ) ) ;
#9503 = CARTESIAN_POINT ( 'NONE',  ( -2.619177996481920179, -3.081379897639443310, 4.272191262657214494 ) ) ;
#9504 = DIRECTION ( 'NONE',  ( -4.794417550286630491E-31, 1.000000000000000000, 1.774290917998389804E-45 ) ) ;
#9505 = CARTESIAN_POINT ( 'NONE',  ( -1.889999999999999902, 8.500000000000000000, 2.664535259100379641E-15 ) ) ;
#9506 = CARTESIAN_POINT ( 'NONE',  ( 1.949083719010301197, -5.359745762711870753, 4.055210292801453953 ) ) ;
#9507 = ORIENTED_EDGE ( 'NONE', *, *, #983, .T. ) ;
#9508 = CARTESIAN_POINT ( 'NONE',  ( -1.899999999999999911, 8.500000000000000000, 0.6099999999999999867 ) ) ;
#9509 = LINE ( 'NONE', #4214, #4092 ) ;
#9510 = CARTESIAN_POINT ( 'NONE',  ( -1.399999999999999911, -8.000000000000000000, 3.299999999999999822 ) ) ;
#9511 = VERTEX_POINT ( 'NONE', #6522 ) ;
#9512 = CARTESIAN_POINT ( 'NONE',  ( -2.318251751302029984, -5.533262711864409766, 4.294764266798999586 ) ) ;
#9513 = CARTESIAN_POINT ( 'NONE',  ( 0.6672256841321406728, -4.152641158900696183, 7.268642361138727637 ) ) ;
#9514 = CARTESIAN_POINT ( 'NONE',  ( 0.009452039534068971960, -5.000193177104105047, 2.350000000173209536 ) ) ;
#9515 = CARTESIAN_POINT ( 'NONE',  ( -2.161103922260861232, -3.496728210468663889, 3.159628768708461877 ) ) ;
#9516 = EDGE_CURVE ( 'NONE', #4993, #14289, #14863, .T. ) ;
#9517 = CARTESIAN_POINT ( 'NONE',  ( 0.1749999999999999889, 8.200000000000001066, 0.4000000000000000222 ) ) ;
#9518 = CARTESIAN_POINT ( 'NONE',  ( 1.886482464143609095, -0.5895330507926000996, 3.890008792968652429 ) ) ;
#9519 = CARTESIAN_POINT ( 'NONE',  ( 1.534924416212170017, -5.333856471232000018, 2.911460733964629899 ) ) ;
#9520 = CARTESIAN_POINT ( 'NONE',  ( 8.785293332290788772E-16, 10.80000000000000071, 7.599999999999999645 ) ) ;
#9521 = ORIENTED_EDGE ( 'NONE', *, *, #17153, .T. ) ;
#9522 = CARTESIAN_POINT ( 'NONE',  ( 1.000000000000000000, -7.000000000000000000, 5.700000000000000178 ) ) ;
#9523 = CARTESIAN_POINT ( 'NONE',  ( 2.353194804772640314, -0.3756355932203400139, 4.731327187377229571 ) ) ;
#9524 = CARTESIAN_POINT ( 'NONE',  ( 1.480680413335799805, -1.214475958216410190, 6.529298007719799735 ) ) ;
#9525 = CARTESIAN_POINT ( 'NONE',  ( -2.234315482767910144, -0.5402542372881360411, 3.960850823455329905 ) ) ;
#9526 = DIRECTION ( 'NONE',  ( 2.168404344971006896E-16, -1.000000000000000000, 0.000000000000000000 ) ) ;
#9527 = EDGE_LOOP ( 'NONE', ( #4645, #18217, #7285, #17020 ) ) ;
#9528 = ADVANCED_FACE ( 'NONE', ( #975 ), #13466, .T. ) ;
#9529 = CARTESIAN_POINT ( 'NONE',  ( 1.899999999999999911, 4.700000000000000178, 0.6099999999999999867 ) ) ;
#9530 = ORIENTED_EDGE ( 'NONE', *, *, #4277, .T. ) ;
#9531 = CARTESIAN_POINT ( 'NONE',  ( 1.943632316591229481, -5.046398305084738745, 3.373048379518160722 ) ) ;
#9532 = DIRECTION ( 'NONE',  ( -1.000000000000000000, 0.000000000000000000, 0.000000000000000000 ) ) ;
#9533 = DIRECTION ( 'NONE',  ( -1.000000000000000000, 0.000000000000000000, 0.000000000000000000 ) ) ;
#9534 = VERTEX_POINT ( 'NONE', #783 ) ;
#9535 = CARTESIAN_POINT ( 'NONE',  ( -0.6864473529425049181, -4.591277760018209975, 6.951118770549909343 ) ) ;
#9536 = ADVANCED_FACE ( 'NONE', ( #14958 ), #6420, .T. ) ;
#9537 = DIRECTION ( 'NONE',  ( -0.7071067811865480168, -1.847167598451501182E-16, 0.7071067811865470176 ) ) ;
#9538 = CARTESIAN_POINT ( 'NONE',  ( 1.550000000000000044, -5.599999999999999645, 5.100000000000000533 ) ) ;
#9539 = CIRCLE ( 'NONE', #15030, 0.04999999999999969746 ) ;
#9540 = CARTESIAN_POINT ( 'NONE',  ( 0.9000000000000000222, 2.050000000000000266, 3.600000000000000089 ) ) ;
#9541 = DIRECTION ( 'NONE',  ( 1.000000000000000000, 0.000000000000000000, 0.000000000000000000 ) ) ;
#9542 = CARTESIAN_POINT ( 'NONE',  ( -2.159566522375440112, -3.240557039297490061, 5.635424033751089468 ) ) ;
#9543 = DIRECTION ( 'NONE',  ( 0.000000000000000000, 0.000000000000000000, 1.000000000000000000 ) ) ;
#9544 = CARTESIAN_POINT ( 'NONE',  ( -2.041954431566909367, -1.750106588847040845, 4.912894203848660268 ) ) ;
#9545 = DIRECTION ( 'NONE',  ( 1.000000000000000000, -2.220446049250309876E-16, -1.048990684667790150E-15 ) ) ;
#9546 = CARTESIAN_POINT ( 'NONE',  ( -0.8244235255442939891, -0.5829339996946389935, 2.492493020344019872 ) ) ;
#9547 = ORIENTED_EDGE ( 'NONE', *, *, #4613, .F. ) ;
#9548 = LINE ( 'NONE', #5007, #1342 ) ;
#9549 = VECTOR ( 'NONE', #3845, 1000.000000000000000 ) ;
#9550 = EDGE_LOOP ( 'NONE', ( #2117, #12812, #4167, #17410 ) ) ;
#9551 = UNCERTAINTY_MEASURE_WITH_UNIT (LENGTH_MEASURE( 1.000000000000000082E-05 ), #1746, 'distance_accuracy_value', 'NONE');
#9552 = ORIENTED_EDGE ( 'NONE', *, *, #2918, .F. ) ;
#9553 = DIRECTION ( 'NONE',  ( 0.000000000000000000, 0.000000000000000000, 1.000000000000000000 ) ) ;
#9554 = CARTESIAN_POINT ( 'NONE',  ( 2.351526912647309953, -5.073093220338979137, 4.606040641882800379 ) ) ;
#9555 = DIRECTION ( 'NONE',  ( 8.971499188890150495E-16, 0.000000000000000000, 1.000000000000000000 ) ) ;
#9556 = DIRECTION ( 'NONE',  ( -1.000000000000000000, -4.336808689942016947E-15, 1.084202172485504276E-14 ) ) ;
#9557 = ORIENTED_EDGE ( 'NONE', *, *, #8132, .T. ) ;
#9558 = CARTESIAN_POINT ( 'NONE',  ( -1.728413393879669968, -1.288181699441249828, 6.297289212178331042 ) ) ;
#9559 = DIRECTION ( 'NONE',  ( 4.707398764864359324E-46, -1.000000000000000000, -2.220446049250309876E-16 ) ) ;
#9560 = CARTESIAN_POINT ( 'NONE',  ( 1.803891155489780074, -0.8185750573155089471, 3.188470185434109982 ) ) ;
#9561 = CARTESIAN_POINT ( 'NONE',  ( 2.353194804772640314, -0.07563559322033940047, 4.731327187377229571 ) ) ;
#9562 = ORIENTED_EDGE ( 'NONE', *, *, #2371, .T. ) ;
#9563 = CARTESIAN_POINT ( 'NONE',  ( 2.180207327701309872, -0.3934322033898309812, 5.586116916730190063 ) ) ;
#9564 = CARTESIAN_POINT ( 'NONE',  ( -2.050059171113549183, -0.5224576271186435195, 4.809263467226075228 ) ) ;
#9565 = ORIENTED_EDGE ( 'NONE', *, *, #4091, .F. ) ;
#9566 = CARTESIAN_POINT ( 'NONE',  ( -2.431060148753501515, -0.2447033898305090438, 3.635668498923334102 ) ) ;
#9567 = VERTEX_POINT ( 'NONE', #2374 ) ;
#9568 = CARTESIAN_POINT ( 'NONE',  ( -0.1749999999999999889, 7.700000000000000178, 1.600000000000000089 ) ) ;
#9569 = VECTOR ( 'NONE', #11825, 1000.000000000000000 ) ;
#9570 = CARTESIAN_POINT ( 'NONE',  ( -0.3949552299395130417, -1.823812330071880261, 2.379923265530350385 ) ) ;
#9571 = CARTESIAN_POINT ( 'NONE',  ( -0.1641805561540918557, -0.5962015548080631389, 2.650681144176719961 ) ) ;
#9572 = CARTESIAN_POINT ( 'NONE',  ( -2.293791554891330353, -4.777584066324515710, 6.034778631725542297 ) ) ;
#9573 = ORIENTED_EDGE ( 'NONE', *, *, #14566, .T. ) ;
#9574 = CARTESIAN_POINT ( 'NONE',  ( -0.009452110982656879157, -5.299807955295460005, 2.350000000000000089 ) ) ;
#9575 = CARTESIAN_POINT ( 'NONE',  ( 0.5902886515193200845, -4.152641158900699736, 6.978224088050040130 ) ) ;
#9576 = CARTESIAN_POINT ( 'NONE',  ( 1.940935473245969156, -0.5041426604022095637, 2.893832807158179143 ) ) ;
#9577 = DIRECTION ( 'NONE',  ( 0.7071067811865470176, -0.7071067811865480168, 0.000000000000000000 ) ) ;
#9578 = CARTESIAN_POINT ( 'NONE',  ( 2.500000000000000000, 7.299999999999999822, 1.600000000000000089 ) ) ;
#9579 = DIRECTION ( 'NONE',  ( -1.000000000000000000, 0.000000000000000000, 0.000000000000000000 ) ) ;
#9580 = CARTESIAN_POINT ( 'NONE',  ( 1.945780800405119360, -0.9117282104686613708, 4.045142061754263274 ) ) ;
#9581 = LINE ( 'NONE', #13747, #6728 ) ;
#9582 = ORIENTED_EDGE ( 'NONE', *, *, #1005, .F. ) ;
#9583 = CARTESIAN_POINT ( 'NONE',  ( 2.500000000000000000, 3.500000000000000000, 0.6099999999999999867 ) ) ;
#9584 = CARTESIAN_POINT ( 'NONE',  ( -1.889999999999999902, 3.500000000000000000, -6.080658959840581147E-16 ) ) ;
#9585 = EDGE_CURVE ( 'NONE', #11828, #18124, #12090, .T. ) ;
#9586 = CARTESIAN_POINT ( 'NONE',  ( 2.589141052314449354, -2.312866384125929820, 5.282633936723466483 ) ) ;
#9587 = ORIENTED_EDGE ( 'NONE', *, *, #881, .F. ) ;
#9588 = CARTESIAN_POINT ( 'NONE',  ( -0.8298945877350979439, -5.211074464177370302, 2.494426474263899962 ) ) ;
#9589 = CARTESIAN_POINT ( 'NONE',  ( 1.432215783582721613, -5.413135593220339992, 6.170863372171116801 ) ) ;
#9590 = ORIENTED_EDGE ( 'NONE', *, *, #14135, .F. ) ;
#9591 = EDGE_CURVE ( 'NONE', #6773, #15430, #16430, .T. ) ;
#9592 = CARTESIAN_POINT ( 'NONE',  ( -1.399999999999999911, -9.500000000000000000, 6.100000000000000533 ) ) ;
#9593 = ADVANCED_FACE ( 'NONE', ( #16338 ), #3642, .T. ) ;
#9594 = LINE ( 'NONE', #8397, #8815 ) ;
#9595 = DIRECTION ( 'NONE',  ( 0.000000000000000000, -1.000000000000000000, 0.000000000000000000 ) ) ;
#9596 = EDGE_CURVE ( 'NONE', #796, #5745, #9122, .T. ) ;
#9597 = ORIENTED_EDGE ( 'NONE', *, *, #2414, .T. ) ;
#9598 = CARTESIAN_POINT ( 'NONE',  ( 2.043308330018790198, -5.399788135593220240, 5.867646457774659652 ) ) ;
#9599 = CARTESIAN_POINT ( 'NONE',  ( -2.022685914314908739, -4.432100618360157007, 6.418096442297106741 ) ) ;
#9600 = CARTESIAN_POINT ( 'NONE',  ( -1.650842931266140790, -3.566593075333521767, 2.622060802311461547 ) ) ;
#9601 = CARTESIAN_POINT ( 'NONE',  ( -1.899999999999999911, 0.7211102550927970256, 4.000000000000000000 ) ) ;
#9602 = CARTESIAN_POINT ( 'NONE',  ( -0.7205524543785096769, -1.171740257999810852, 6.622421910798247602 ) ) ;
#9603 = CARTESIAN_POINT ( 'NONE',  ( 2.500000000000000000, 7.299999999999999822, 1.600000000000000089 ) ) ;
#9604 = CARTESIAN_POINT ( 'NONE',  ( 1.899999999999999911, 10.00000000000000000, -7.696722944179978717E-16 ) ) ;
#9605 = ORIENTED_EDGE ( 'NONE', *, *, #11308, .F. ) ;
#9606 = LINE ( 'NONE', #6920, #3493 ) ;
#9607 = CARTESIAN_POINT ( 'NONE',  ( 0.1565249325564390115, -0.4468220338983060480, 7.048192310558509810 ) ) ;
#9608 = CARTESIAN_POINT ( 'NONE',  ( -2.137408332595969629, -3.450151633892079683, 3.714996798363980002 ) ) ;
#9609 = CARTESIAN_POINT ( 'NONE',  ( 1.899999999999999911, 2.000000000000000000, -1.522591576628789972E-15 ) ) ;
#9610 = DIRECTION ( 'NONE',  ( 1.000000000000000000, 1.224646799147350002E-16, 0.000000000000000000 ) ) ;
#9611 = CARTESIAN_POINT ( 'NONE',  ( 1.031876288691629506, -5.430932203389830626, 7.145012538880298081 ) ) ;
#9612 = VERTEX_POINT ( 'NONE', #12179 ) ;
#9613 = VECTOR ( 'NONE', #11708, 1000.000000000000000 ) ;
#9614 = EDGE_CURVE ( 'NONE', #16401, #2785, #16535, .T. ) ;
#9615 = VERTEX_POINT ( 'NONE', #14836 ) ;
#9616 = CARTESIAN_POINT ( 'NONE',  ( 0.7093417302541467073, -5.135381355932199021, 6.943956659919690466 ) ) ;
#9617 = DIRECTION ( 'NONE',  ( -0.7071067811865475727, 0.7071067811865475727, 0.000000000000000000 ) ) ;
#9618 = DIRECTION ( 'NONE',  ( 1.060879779086260081E-14, -8.223874256482640091E-16, 1.000000000000000000 ) ) ;
#9619 = ORIENTED_EDGE ( 'NONE', *, *, #11390, .T. ) ;
#9620 = CARTESIAN_POINT ( 'NONE',  ( -2.036228139452650243, -3.473439922180369788, 3.519948877554409883 ) ) ;
#9621 =( LENGTH_UNIT ( ) NAMED_UNIT ( * ) SI_UNIT ( .MILLI., .METRE. ) );
#9622 = CARTESIAN_POINT ( 'NONE',  ( 1.319613955262860072, -5.028306595106929677, 2.740497729816110173 ) ) ;
#9623 = CARTESIAN_POINT ( 'NONE',  ( 2.500000000000000000, 11.29999999999999893, 1.600000000000000089 ) ) ;
#9624 = CARTESIAN_POINT ( 'NONE',  ( -1.699999999999999956, 9.299999999999998934, 7.599999999999999645 ) ) ;
#9625 = CARTESIAN_POINT ( 'NONE',  ( 1.353103843060669886, -2.798079561820010053, 6.625579309552930063 ) ) ;
#9626 = CARTESIAN_POINT ( 'NONE',  ( 3.673940397442050254E-17, 2.600000000000000089, 8.000000000000000000 ) ) ;
#9627 = CARTESIAN_POINT ( 'NONE',  ( -1.883235269974520287, -3.240557039297494057, 5.517512544583926370 ) ) ;
#9628 = DIRECTION ( 'NONE',  ( -5.734623061080349568E-18, 0.000000000000000000, 1.000000000000000000 ) ) ;
#9629 = PLANE ( 'NONE',  #13000 ) ;
#9630 = ORIENTED_EDGE ( 'NONE', *, *, #13329, .T. ) ;
#9631 = ADVANCED_FACE ( 'NONE', ( #11594 ), #17223, .T. ) ;
#9632 = ORIENTED_EDGE ( 'NONE', *, *, #15381, .T. ) ;
#9633 = VERTEX_POINT ( 'NONE', #14348 ) ;
#9634 = ORIENTED_EDGE ( 'NONE', *, *, #3826, .F. ) ;
#9635 = CARTESIAN_POINT ( 'NONE',  ( -1.255262969126040791E-16, 2.049999999999999822, 5.100000000000000533 ) ) ;
#9636 = CARTESIAN_POINT ( 'NONE',  ( 0.05465110135556765225, -5.148728813559319661, 6.752241303418941243 ) ) ;
#9637 = PRODUCT ( 'Switch Metal Shield Frame', 'Switch Metal Shield Frame', '', ( #10037 ) ) ;
#9638 = CARTESIAN_POINT ( 'NONE',  ( -1.152986057740030379, -1.753947465207011058, 2.309657588616440549 ) ) ;
#9639 = AXIS2_PLACEMENT_3D ( 'NONE', #8064, #17931, #10927 ) ;
#9640 = CARTESIAN_POINT ( 'NONE',  ( -6.735557395310430190E-17, 7.000000000000000000, 6.299999999999999822 ) ) ;
#9641 = DIRECTION ( 'NONE',  ( 1.000000000000000000, 0.000000000000000000, 0.000000000000000000 ) ) ;
#9642 = DIRECTION ( 'NONE',  ( 1.224510688924809779E-16, -1.000000000000000000, -1.306144734853129823E-16 ) ) ;
#9643 = LINE ( 'NONE', #17031, #14979 ) ;
#9644 = LINE ( 'NONE', #13992, #12887 ) ;
#9645 = AXIS2_PLACEMENT_3D ( 'NONE', #7870, #17760, #16391 ) ;
#9646 = DIRECTION ( 'NONE',  ( 1.000000000000000000, 0.000000000000000000, 0.000000000000000000 ) ) ;
#9647 = CARTESIAN_POINT ( 'NONE',  ( -0.1569242594330230167, -1.400782264522720144, 7.048216443236290374 ) ) ;
#9648 = CARTESIAN_POINT ( 'NONE',  ( 1.707817112497189926, -0.1112288135593230004, 6.319218296629480314 ) ) ;
#9649 = ORIENTED_EDGE ( 'NONE', *, *, #1028, .T. ) ;
#9650 = CARTESIAN_POINT ( 'NONE',  ( -2.332582362116870200, -0.5313559322033900578, 4.387643303570819775 ) ) ;
#9651 = EDGE_LOOP ( 'NONE', ( #10959, #14375, #14160, #12591 ) ) ;
#9652 = CARTESIAN_POINT ( 'NONE',  ( -2.304156201936080617, -0.2002118644067801267, 6.016707707703351282 ) ) ;
#9653 = CARTESIAN_POINT ( 'NONE',  ( -1.899999999999999911, 0.5999999999999999778, 7.599999999999999645 ) ) ;
#9654 = EDGE_LOOP ( 'NONE', ( #11976, #9712, #4424 ) ) ;
#9655 = DIRECTION ( 'NONE',  ( -1.000000000000000000, 2.220446049250309876E-16, 0.000000000000000000 ) ) ;
#9656 = CARTESIAN_POINT ( 'NONE',  ( 0.09706517602699295255, -2.638902420161969076, 7.051451474958978061 ) ) ;
#9657 = DIRECTION ( 'NONE',  ( 0.000000000000000000, 0.000000000000000000, 1.000000000000000000 ) ) ;
#9658 = CARTESIAN_POINT ( 'NONE',  ( 1.851400890972779045, -5.413135593220339992, 6.601359968904126241 ) ) ;
#9659 = VERTEX_POINT ( 'NONE', #14619 ) ;
#9660 = DIRECTION ( 'NONE',  ( 1.000000000000000000, -2.220446049250319983E-16, 0.000000000000000000 ) ) ;
#9661 = CARTESIAN_POINT ( 'NONE',  ( -0.4985810152601130585, -4.269082600342140488, 7.000035360316470445 ) ) ;
#9662 = AXIS2_PLACEMENT_3D ( 'NONE', #5622, #7276, #4402 ) ;
#9663 = CARTESIAN_POINT ( 'NONE',  ( 0.4500319419456214609, -4.474836318576761229, 7.315451193241913508 ) ) ;
#9664 = DIRECTION ( 'NONE',  ( 7.401486830834370362E-16, 0.000000000000000000, 1.000000000000000000 ) ) ;
#9665 = DIRECTION ( 'NONE',  ( 0.2800000000000001377, -0.9599999999999999645, 0.000000000000000000 ) ) ;
#9666 = CARTESIAN_POINT ( 'NONE',  ( 0.5500000000000000444, 6.450000000000000178, 3.600000000000000089 ) ) ;
#9667 = CARTESIAN_POINT ( 'NONE',  ( -2.052909741356249373, -1.773394877135329839, 4.721527574705180363 ) ) ;
#9668 = CARTESIAN_POINT ( 'NONE',  ( -0.5500000000000000444, 6.450000000000000178, 3.200000000000000178 ) ) ;
#9669 = AXIS2_PLACEMENT_3D ( 'NONE', #3670, #8131, #2202 ) ;
#9670 = VERTEX_POINT ( 'NONE', #1674 ) ;
#9671 = CARTESIAN_POINT ( 'NONE',  ( -1.399999999999999911, 5.799999999999999822, 7.700000000000000178 ) ) ;
#9672 = STYLED_ITEM ( 'NONE', ( #3065 ), #14083 ) ;
#9673 = CARTESIAN_POINT ( 'NONE',  ( 2.241103642439659443E-15, 9.099999999999999645, 7.700000000000000178 ) ) ;
#9674 = CARTESIAN_POINT ( 'NONE',  ( -2.051331987628511211, -0.2269067796610169385, 4.618035453557344461 ) ) ;
#9675 = CARTESIAN_POINT ( 'NONE',  ( -1.428323476796611535, -3.290974492234041815, 2.463260019887531627 ) ) ;
#9676 = COLOUR_RGB ( '', 0.72549020, 0.75294118, 0.79215686) ;
#9677 = CARTESIAN_POINT ( 'NONE',  ( 0.009452110982653675123, -5.000192044704546035, 2.649999999999998579 ) ) ;
#9678 = CARTESIAN_POINT ( 'NONE',  ( -0.9222751404131093178, -5.277754237288146300, 2.865854510788139908 ) ) ;
#9679 = ORIENTED_EDGE ( 'NONE', *, *, #3473, .F. ) ;
#9680 = CARTESIAN_POINT ( 'NONE',  ( 0.2335786437626899970, 6.450000000000000178, 1.958578643762689753 ) ) ;
#9681 = FACE_OUTER_BOUND ( 'NONE', #10885, .T. ) ;
#9682 = DIRECTION ( 'NONE',  ( -1.224646799147341128E-16, -1.000000000000000000, 0.000000000000000000 ) ) ;
#9683 = ORIENTED_EDGE ( 'NONE', *, *, #9255, .F. ) ;
#9684 = VECTOR ( 'NONE', #6611, 1000.000000000000000 ) ;
#9685 = CARTESIAN_POINT ( 'NONE',  ( -2.116444151961480280, -5.546610169491529518, 3.670839500609359707 ) ) ;
#9686 = AXIS2_PLACEMENT_3D ( 'NONE', #4132, #15361, #6915 ) ;
#9687 = CARTESIAN_POINT ( 'NONE',  ( 2.161802606005190253, -0.5895330507925999886, 3.769755311421790545 ) ) ;
#9688 = CARTESIAN_POINT ( 'NONE',  ( -2.409576349373780513, -3.450151633892079239, 3.587770028483140194 ) ) ;
#9689 = CARTESIAN_POINT ( 'NONE',  ( -0.3750000000000000000, 3.050000000000000266, 2.100000000000000089 ) ) ;
#9690 = CARTESIAN_POINT ( 'NONE',  ( -1.704669856830349994, -4.796950468210010143, 3.080704711052660194 ) ) ;
#9691 = AXIS2_PLACEMENT_3D ( 'NONE', #9128, #712, #2295 ) ;
#9692 =( REPRESENTATION_RELATIONSHIP ('NONE','NONE', #2757, #4513 ) REPRESENTATION_RELATIONSHIP_WITH_TRANSFORMATION ( #13538 )SHAPE_REPRESENTATION_RELATIONSHIP( ) );
#9693 = EDGE_CURVE ( 'NONE', #5609, #8437, #11661, .T. ) ;
#9694 = VECTOR ( 'NONE', #11341, 1000.000000000000000 ) ;
#9695 = CARTESIAN_POINT ( 'NONE',  ( -0.3042893218813459977, 6.450000000000000178, 2.029289321881350361 ) ) ;
#9696 = EDGE_LOOP ( 'NONE', ( #17531, #12914, #5948, #17969 ) ) ;
#9697 = EDGE_CURVE ( 'NONE', #8719, #1735, #7323, .T. ) ;
#9698 = AXIS2_PLACEMENT_3D ( 'NONE', #12183, #8113, #6715 ) ;
#9699 = CARTESIAN_POINT ( 'NONE',  ( -1.850000000000000089, -6.000000000000000000, 6.400000000000000355 ) ) ;
#9700 = CARTESIAN_POINT ( 'NONE',  ( -1.943632316591239917, -0.5536016949152539057, 3.373048379518170048 ) ) ;
#9701 = CARTESIAN_POINT ( 'NONE',  ( -1.286937324407759986, -3.589881363621809651, 2.729584305145209999 ) ) ;
#9702 = CARTESIAN_POINT ( 'NONE',  ( 0.1749999999999999889, 7.500000000000000000, 3.100000000000000089 ) ) ;
#9703 = FACE_OUTER_BOUND ( 'NONE', #10732, .T. ) ;
#9704 = CARTESIAN_POINT ( 'NONE',  ( -0.9664230948142090716, -5.582203389830510787, 2.228384861502259895 ) ) ;
#9705 = ORIENTED_EDGE ( 'NONE', *, *, #11156, .F. ) ;
#9706 = ORIENTED_EDGE ( 'NONE', *, *, #5696, .F. ) ;
#9707 = DIRECTION ( 'NONE',  ( 1.184237892933500047E-15, -1.000000000000000000, 0.000000000000000000 ) ) ;
#9708 = DIRECTION ( 'NONE',  ( -9.588835100573269740E-31, 1.000000000000000000, 3.548581835996780230E-45 ) ) ;
#9709 =( NAMED_UNIT ( * ) SI_UNIT ( $, .STERADIAN. ) SOLID_ANGLE_UNIT ( ) );
#9710 = LINE ( 'NONE', #18108, #9101 ) ;
#9711 = AXIS2_PLACEMENT_3D ( 'NONE', #17387, #10360, #6277 ) ;
#9712 = ORIENTED_EDGE ( 'NONE', *, *, #14472, .T. ) ;
#9713 = CARTESIAN_POINT ( 'NONE',  ( -1.777964140657649850, -4.731007489747940831, 6.241943319976260618 ) ) ;
#9714 = VECTOR ( 'NONE', #18001, 1000.000000000000000 ) ;
#9715 = EDGE_CURVE ( 'NONE', #9633, #3220, #8706, .T. ) ;
#9716 = CARTESIAN_POINT ( 'NONE',  ( 0.2270348434643680025, -5.304612347394249916, 2.348896311281980065 ) ) ;
#9717 = CARTESIAN_POINT ( 'NONE',  ( -1.000000000000000000, -6.000000000000000000, 3.299999999999999822 ) ) ;
#9718 = EDGE_CURVE ( 'NONE', #12326, #8282, #1769, .T. ) ;
#9719 = CARTESIAN_POINT ( 'NONE',  ( -1.889999999999999902, 4.700000000000000178, 0.6099999999999999867 ) ) ;
#9720 = CARTESIAN_POINT ( 'NONE',  ( 2.353452300571019506, -4.125511994252439862, 4.697179287168359529 ) ) ;
#9721 = EDGE_CURVE ( 'NONE', #4438, #12426, #14536, .T. ) ;
#9722 = VECTOR ( 'NONE', #5390, 1000.000000000000000 ) ;
#9723 = CARTESIAN_POINT ( 'NONE',  ( -1.652654650382402668, -4.804713230972782689, 3.029252778805632484 ) ) ;
#9724 = VECTOR ( 'NONE', #5761, 1000.000000000000000 ) ;
#9725 = CARTESIAN_POINT ( 'NONE',  ( 0.1526488871098231337, -3.752899381639833720, 2.652660223633551251 ) ) ;
#9726 = CARTESIAN_POINT ( 'NONE',  ( -0.2812789908084309953, -0.4557203389830509765, 7.036533610117280624 ) ) ;
#9727 = CARTESIAN_POINT ( 'NONE',  ( -1.836970198721025435E-17, 5.318248954186070243, 6.850000000000000533 ) ) ;
#9728 = VERTEX_POINT ( 'NONE', #3402 ) ;
#9729 = LINE ( 'NONE', #4164, #4711 ) ;
#9730 = ORIENTED_EDGE ( 'NONE', *, *, #11085, .T. ) ;
#9731 = AXIS2_PLACEMENT_3D ( 'NONE', #4281, #222, #127 ) ;
#9732 = DIRECTION ( 'NONE',  ( -1.000000000000000000, 0.000000000000000000, 0.000000000000000000 ) ) ;
#9733 = ORIENTED_EDGE ( 'NONE', *, *, #1598, .T. ) ;
#9734 = ORIENTED_EDGE ( 'NONE', *, *, #9242, .T. ) ;
#9735 = UNCERTAINTY_MEASURE_WITH_UNIT (LENGTH_MEASURE( 1.000000000000000082E-05 ), #1648, 'distance_accuracy_value', 'NONE');
#9736 = ORIENTED_EDGE ( 'NONE', *, *, #13267, .F. ) ;
#9737 = EDGE_CURVE ( 'NONE', #12188, #2390, #17285, .T. ) ;
#9738 = CARTESIAN_POINT ( 'NONE',  ( 1.149999999999999911, 9.299999999999998934, 7.700000000000000178 ) ) ;
#9739 = AXIS2_PLACEMENT_3D ( 'NONE', #15862, #13081, #6198 ) ;
#9740 = CARTESIAN_POINT ( 'NONE',  ( -0.1365430262726299304, -5.153177966101685215, 6.748423079423377047 ) ) ;
#9741 = CARTESIAN_POINT ( 'NONE',  ( -2.607432201095288615, -1.521064582324129777, 4.205620581240213873 ) ) ;
#9742 = CARTESIAN_POINT ( 'NONE',  ( 2.616666666666660035, -5.805074450128190455E-17, 4.000000000000000000 ) ) ;
#9743 = DIRECTION ( 'NONE',  ( 0.000000000000000000, -1.000000000000000000, 0.000000000000000000 ) ) ;
#9744 = CARTESIAN_POINT ( 'NONE',  ( 0.000000000000000000, 4.930380657631319405E-32, 8.300000000000000711 ) ) ;
#9745 = ADVANCED_FACE ( 'NONE', ( #6100 ), #11763, .F. ) ;
#9746 = CARTESIAN_POINT ( 'NONE',  ( 0.5500000000000000444, 2.050000000000000266, 3.600000000000000089 ) ) ;
#9747 = CARTESIAN_POINT ( 'NONE',  ( 2.231116159141619981, -0.9117282104686620370, 3.951089877392439664 ) ) ;
#9748 = CARTESIAN_POINT ( 'NONE',  ( -0.2993653819235400082, -2.685478996738538626, 6.731079075450757898 ) ) ;
#9749 = CARTESIAN_POINT ( 'NONE',  ( 0.9222751404130974384, -0.02224576271186471527, 2.865854510788131027 ) ) ;
#9750 = CARTESIAN_POINT ( 'NONE',  ( -1.112838723655040107, -0.4735169491525429986, 6.773667561836210105 ) ) ;
#9751 = VECTOR ( 'NONE', #9579, 1000.000000000000000 ) ;
#9752 = VERTEX_POINT ( 'NONE', #6081 ) ;
#9753 = CARTESIAN_POINT ( 'NONE',  ( 0.7983658734558030101, -0.1334745762711870010, 6.913847129767330735 ) ) ;
#9754 = CARTESIAN_POINT ( 'NONE',  ( 1.644832646965660006, -1.191187669928119863, 6.383232381746459794 ) ) ;
#9755 = VERTEX_POINT ( 'NONE', #11465 ) ;
#9756 = CARTESIAN_POINT ( 'NONE',  ( 2.616666666666660035, -5.805074450128190455E-17, 4.000000000000000000 ) ) ;
#9757 = VERTEX_POINT ( 'NONE', #2001 ) ;
#9758 = ADVANCED_FACE ( 'NONE', ( #7397 ), #13036, .T. ) ;
#9759 = CARTESIAN_POINT ( 'NONE',  ( -1.567709126316399804, -1.684082600342149627, 2.944712621036611022 ) ) ;
#9760 = CARTESIAN_POINT ( 'NONE',  ( -2.601107615185130673, -5.515466101694915579, 5.226397344856384741 ) ) ;
#9761 = ORIENTED_EDGE ( 'NONE', *, *, #9137, .T. ) ;
#9762 = EDGE_CURVE ( 'NONE', #14900, #15707, #10241, .T. ) ;
#9763 = CARTESIAN_POINT ( 'NONE',  ( -2.182690844914350059, -1.680241723982170088, 5.580117243900479806 ) ) ;
#9764 = EDGE_CURVE ( 'NONE', #7970, #5456, #4582, .T. ) ;
#9765 = VECTOR ( 'NONE', #100, 1000.000000000000000 ) ;
#9766 = CARTESIAN_POINT ( 'NONE',  ( 2.052786957354850728, -0.3756355932203404024, 4.727327971967373976 ) ) ;
#9767 = ORIENTED_EDGE ( 'NONE', *, *, #11156, .T. ) ;
#9768 = ADVANCED_FACE ( 'NONE', ( #14517 ), #13569, .T. ) ;
#9769 = LINE ( 'NONE', #15236, #8772 ) ;
#9770 = LINE ( 'NONE', #5418, #9751 ) ;
#9771 = CARTESIAN_POINT ( 'NONE',  ( -2.013199450439951299, -1.726818300558751851, 5.102405038955014405 ) ) ;
#9772 = DIRECTION ( 'NONE',  ( 1.000000000000000000, 4.037174635000560229E-16, 0.000000000000000000 ) ) ;
#9773 = ORIENTED_EDGE ( 'NONE', *, *, #11516, .T. ) ;
#9774 = DIRECTION ( 'NONE',  ( 3.315303352997239924E-31, -1.000000000000000000, 8.588360937600549480E-46 ) ) ;
#9775 = FACE_OUTER_BOUND ( 'NONE', #16340, .T. ) ;
#9776 = CARTESIAN_POINT ( 'NONE',  ( 2.012177589105479392, -0.3845338983050847759, 5.107213040360584877 ) ) ;
#9777 = CARTESIAN_POINT ( 'NONE',  ( -0.7540633504678314614, -3.360839357098899693, 2.155495695330209127 ) ) ;
#9778 = VECTOR ( 'NONE', #10232, 1000.000000000000000 ) ;
#9779 = CARTESIAN_POINT ( 'NONE',  ( -0.5372984490435469551, 4.250000000000000000, 7.700000000000000178 ) ) ;
#9780 = CARTESIAN_POINT ( 'NONE',  ( -1.505092429369619955, -5.128627060139309357, 2.879659483602799774 ) ) ;
#9781 = CARTESIAN_POINT ( 'NONE',  ( 1.795861365445541091, -5.350847457627126325, 3.705232155007893713 ) ) ;
#9782 = ORIENTED_EDGE ( 'NONE', *, *, #2249, .F. ) ;
#9783 = CARTESIAN_POINT ( 'NONE',  ( 0.2189795514005130062, -0.004449152542373159026, 2.356806637999009801 ) ) ;
#9784 = DIRECTION ( 'NONE',  ( 4.485749594445080178E-16, 0.000000000000000000, 1.000000000000000000 ) ) ;
#9785 = CARTESIAN_POINT ( 'NONE',  ( -1.850000000000000089, 11.25000000000000000, 8.300000000000000711 ) ) ;
#9786 = ORIENTED_EDGE ( 'NONE', *, *, #252, .T. ) ;
#9787 = CARTESIAN_POINT ( 'NONE',  ( -1.850000000000000089, -5.599999999999999645, 2.299999999999999822 ) ) ;
#9788 = CARTESIAN_POINT ( 'NONE',  ( -2.516451517878150135, -4.688271789531334832, 3.857037693030694214 ) ) ;
#9789 = CARTESIAN_POINT ( 'NONE',  ( 0.5500000000000000444, 6.450000000000000178, 2.699264068711930253 ) ) ;
#9790 = VECTOR ( 'NONE', #7134, 1000.000000000000000 ) ;
#9791 = CARTESIAN_POINT ( 'NONE',  ( -1.974086094277271108, -1.404623140882690580, 5.263813741415750869 ) ) ;
#9792 = DIRECTION ( 'NONE',  ( -1.000000000000000000, 0.000000000000000000, 7.401486830834380223E-16 ) ) ;
#9793 = ORIENTED_EDGE ( 'NONE', *, *, #10841, .T. ) ;
#9794 = EDGE_CURVE ( 'NONE', #8080, #5857, #16088, .T. ) ;
#9795 = CARTESIAN_POINT ( 'NONE',  ( 1.000000000000000000, -5.599999999999999645, 3.673738709727309981 ) ) ;
#9796 = CARTESIAN_POINT ( 'NONE',  ( 1.610878918935058524, -0.3311440677966099311, 2.590989782159081933 ) ) ;
#9797 = CARTESIAN_POINT ( 'NONE',  ( -0.3159454637156809409, -2.984385868126319785, 7.032150113402090064 ) ) ;
#9798 = DIRECTION ( 'NONE',  ( 0.000000000000000000, 1.000000000000000000, 0.000000000000000000 ) ) ;
#9799 = DIRECTION ( 'NONE',  ( -1.387778780781439759E-16, -1.110223024625160090E-15, -1.000000000000000000 ) ) ;
#9800 = CARTESIAN_POINT ( 'NONE',  ( -0.4917262214559124933, -5.591101694915256104, 2.092115739186370948 ) ) ;
#9801 = EDGE_LOOP ( 'NONE', ( #4813, #17671, #6926, #15590 ) ) ;
#9802 = PRODUCT_DEFINITION_SHAPE ( 'NONE', 'NONE',  #14462 ) ;
#9803 = ORIENTED_EDGE ( 'NONE', *, *, #1896, .F. ) ;
#9804 = CARTESIAN_POINT ( 'NONE',  ( -1.899999999999999911, 7.299999999999999822, 1.600000000000000089 ) ) ;
#9805 = SHAPE_REPRESENTATION_RELATIONSHIP ( 'NONE' , 'NONE' ,  #16473, #4658 ) ;
#9806 = LINE ( 'NONE', #9989, #8236 ) ;
#9807 = ORIENTED_EDGE ( 'NONE', *, *, #8991, .F. ) ;
#9808 = EDGE_CURVE ( 'NONE', #13413, #17808, #17537, .T. ) ;
#9809 = CARTESIAN_POINT ( 'NONE',  ( 2.426866425021050766, -0.8884399221803740421, 3.626019996130599665 ) ) ;
#9810 = CARTESIAN_POINT ( 'NONE',  ( 0.5637478356992829953, -0.6606104644819250638, 2.398845082743519708 ) ) ;
#9811 = CARTESIAN_POINT ( 'NONE',  ( 0.2570708662023959423, -5.304612347394245475, 2.048876625919409111 ) ) ;
#9812 = CARTESIAN_POINT ( 'NONE',  ( -1.899999999999999911, 11.40000000000000036, 6.599999999999999645 ) ) ;
#9813 = DIRECTION ( 'NONE',  ( 0.000000000000000000, 0.000000000000000000, -1.000000000000000000 ) ) ;
#9814 = CARTESIAN_POINT ( 'NONE',  ( -2.135041058613629694, -4.800872354612799597, 5.690123914223820023 ) ) ;
#9815 = DIRECTION ( 'NONE',  ( -1.000000000000000000, 6.098637220230962441E-16, 0.000000000000000000 ) ) ;
#9816 = CARTESIAN_POINT ( 'NONE',  ( 1.333132471082870918, -2.774791273531719060, 6.261300629978916454 ) ) ;
#9817 = CARTESIAN_POINT ( 'NONE',  ( -1.477796163681079911, -0.4824152542372879826, 6.531563725478150673 ) ) ;
#9818 = CARTESIAN_POINT ( 'NONE',  ( -1.889999999999999902, 4.700000000000000178, 0.6099999999999999867 ) ) ;
#9819 = ORIENTED_EDGE ( 'NONE', *, *, #9452, .T. ) ;
#9820 = CARTESIAN_POINT ( 'NONE',  ( 1.899999999999999911, 9.199999999999999289, 1.600000000000000089 ) ) ;
#9821 = EDGE_LOOP ( 'NONE', ( #2089, #2236, #11395, #2789 ) ) ;
#9822 = EDGE_CURVE ( 'NONE', #9877, #8376, #14883, .T. ) ;
#9823 = CARTESIAN_POINT ( 'NONE',  ( -1.899999999999999911, 9.199999999999999289, 1.600000000000000089 ) ) ;
#9824 = ORIENTED_EDGE ( 'NONE', *, *, #10473, .F. ) ;
#9825 = CARTESIAN_POINT ( 'NONE',  ( -1.850000000000000089, 11.25000000000000000, 7.700000000000000178 ) ) ;
#9826 = PRODUCT_RELATED_PRODUCT_CATEGORY ( 'part', '', ( #8021 ) ) ;
#9827 = ADVANCED_FACE ( 'NONE', ( #7658 ), #3480, .T. ) ;
#9828 = ORIENTED_EDGE ( 'NONE', *, *, #13326, .T. ) ;
#9829 = DIRECTION ( 'NONE',  ( 1.306144734853129823E-16, -1.000000000000000000, 0.000000000000000000 ) ) ;
#9830 = EDGE_CURVE ( 'NONE', #13175, #11001, #648, .T. ) ;
#9831 = CARTESIAN_POINT ( 'NONE',  ( 1.795861365445541091, -5.050847457627124726, 3.705232155007893713 ) ) ;
#9832 = EDGE_CURVE ( 'NONE', #10555, #12628, #18080, .T. ) ;
#9833 = CARTESIAN_POINT ( 'NONE',  ( -0.5500000000000000444, 7.799999999999999822, 3.600000000000000089 ) ) ;
#9834 = CARTESIAN_POINT ( 'NONE',  ( 1.899999999999999911, 0.5999999999999999778, 7.700000000000000178 ) ) ;
#9835 = ADVANCED_FACE ( 'NONE', ( #9126 ), #909, .T. ) ;
#9836 = FACE_OUTER_BOUND ( 'NONE', #6848, .T. ) ;
#9837 = DIRECTION ( 'NONE',  ( -0.7049180327868849183, 0.7092887755011130224, 8.531426931033447850E-16 ) ) ;
#9838 = CARTESIAN_POINT ( 'NONE',  ( 2.023259452208809872, -2.425466949207399914, 3.497849062500220096 ) ) ;
#9839 = CARTESIAN_POINT ( 'NONE',  ( -2.025702773739959106, -3.081379897639443310, 4.366188503657674858 ) ) ;
#9840 = CARTESIAN_POINT ( 'NONE',  ( 1.392553072310509510, -0.03559322033898333626, 3.191531554476519261 ) ) ;
#9841 = ORIENTED_EDGE ( 'NONE', *, *, #11335, .F. ) ;
#9842 = AXIS2_PLACEMENT_3D ( 'NONE', #5610, #15618, #11347 ) ;
#9843 = CARTESIAN_POINT ( 'NONE',  ( 1.549742865090599997, -0.4156779661016959948, 6.471102547561449647 ) ) ;
#9844 = CARTESIAN_POINT ( 'NONE',  ( 0.5500000000000000444, 3.050000000000000266, 3.399999999999999911 ) ) ;
#9845 = ORIENTED_EDGE ( 'NONE', *, *, #9159, .T. ) ;
#9846 = CARTESIAN_POINT ( 'NONE',  ( 1.707817112497189926, -0.1112288135593230004, 6.319218296629480314 ) ) ;
#9847 = CARTESIAN_POINT ( 'NONE',  ( 1.704669856830330010, -0.8030495317899829510, 3.080704711052640210 ) ) ;
#9848 = ORIENTED_EDGE ( 'NONE', *, *, #9737, .T. ) ;
#9849 = DIRECTION ( 'NONE',  ( 7.273661547324610053E-16, -6.123233995736769734E-17, 1.000000000000000000 ) ) ;
#9850 = EDGE_CURVE ( 'NONE', #9328, #8832, #2942, .T. ) ;
#9851 = ORIENTED_EDGE ( 'NONE', *, *, #5630, .F. ) ;
#9852 = CARTESIAN_POINT ( 'NONE',  ( 2.159566522375459652, -2.359442960702510028, 5.635424033751040618 ) ) ;
#9853 = CARTESIAN_POINT ( 'NONE',  ( -1.057242234132100167, -5.577754237288139905, 2.597442975781530272 ) ) ;
#9854 = ADVANCED_FACE ( 'NONE', ( #995 ), #6547, .F. ) ;
#9855 = ORIENTED_EDGE ( 'NONE', *, *, #2369, .T. ) ;
#9856 = CARTESIAN_POINT ( 'NONE',  ( 1.704669856830330010, -0.8030495317899829510, 3.080704711052640210 ) ) ;
#9857 = CARTESIAN_POINT ( 'NONE',  ( -1.679950111053631900, -0.4957627118644069575, 5.880020650119711867 ) ) ;
#9858 = ORIENTED_EDGE ( 'NONE', *, *, #9955, .F. ) ;
#9859 = DIRECTION ( 'NONE',  ( 1.000000000000000000, 0.000000000000000000, 0.000000000000000000 ) ) ;
#9860 = CARTESIAN_POINT ( 'NONE',  ( 1.899999999999999911, 9.199999999999999289, 0.5999999999999999778 ) ) ;
#9861 = PLANE ( 'NONE',  #1767 ) ;
#9862 = CARTESIAN_POINT ( 'NONE',  ( -2.041954431566909367, -1.750106588847040845, 4.912894203848660268 ) ) ;
#9863 = DIRECTION ( 'NONE',  ( 2.960594732333750117E-16, 1.000000000000000000, 0.000000000000000000 ) ) ;
#9864 = CARTESIAN_POINT ( 'NONE',  ( 2.230812463554230352, -0.4023305084745772420, 6.137473736419911674 ) ) ;
#9865 = ORIENTED_EDGE ( 'NONE', *, *, #6265, .T. ) ;
#9866 = CARTESIAN_POINT ( 'NONE',  ( -1.800000000000000044, 11.40000000000000036, 6.599999999999999645 ) ) ;
#9867 = DIRECTION ( 'NONE',  ( 0.000000000000000000, -1.000000000000000000, 0.000000000000000000 ) ) ;
#9868 = CARTESIAN_POINT ( 'NONE',  ( 2.052786957354850728, -0.3756355932203404024, 4.727327971967373976 ) ) ;
#9869 = AXIS2_PLACEMENT_3D ( 'NONE', #14969, #16258, #18060 ) ;
#9870 = FACE_OUTER_BOUND ( 'NONE', #11547, .T. ) ;
#9871 = CARTESIAN_POINT ( 'NONE',  ( -2.046424002475610404, -5.228813559322024851, 4.536201610417774255 ) ) ;
#9872 = ORIENTED_EDGE ( 'NONE', *, *, #9390, .T. ) ;
#9873 = EDGE_CURVE ( 'NONE', #7939, #11433, #10919, .T. ) ;
#9874 = CARTESIAN_POINT ( 'NONE',  ( -2.500000000000000000, 9.199999999999999289, 0.5999999999999999778 ) ) ;
#9875 = CARTESIAN_POINT ( 'NONE',  ( 2.351526912647309953, -5.373093220338979847, 4.606040641882800379 ) ) ;
#9876 = DIRECTION ( 'NONE',  ( -2.220446049250309876E-16, -1.000000000000000000, -3.286920438420880041E-31 ) ) ;
#9877 = VERTEX_POINT ( 'NONE', #3665 ) ;
#9878 = CARTESIAN_POINT ( 'NONE',  ( -1.500000000000000000, -5.599999999999999645, 2.299999999999999822 ) ) ;
#9879 = CARTESIAN_POINT ( 'NONE',  ( 0.4735094604799090501, -1.032010528270079996, 7.005327412390689901 ) ) ;
#9880 = CARTESIAN_POINT ( 'NONE',  ( 2.200000000000000178, 1.684703763649490251E-16, 7.649999999999999467 ) ) ;
#9881 = CARTESIAN_POINT ( 'NONE',  ( 1.503462833636809881, -0.5041426604022095637, 3.304888304972889657 ) ) ;
#9882 = DIRECTION ( 'NONE',  ( 0.000000000000000000, 0.000000000000000000, 1.000000000000000000 ) ) ;
#9883 = ORIENTED_EDGE ( 'NONE', *, *, #7119, .F. ) ;
#9884 = DIRECTION ( 'NONE',  ( -1.734723475976809806E-16, 1.000000000000000000, 0.000000000000000000 ) ) ;
#9885 = AXIS2_PLACEMENT_3D ( 'NONE', #5663, #9912, #2879 ) ;
#9886 = CARTESIAN_POINT ( 'NONE',  ( -2.224278379903029901, -0.5091101694915259879, 5.468825643806110470 ) ) ;
#9887 = CARTESIAN_POINT ( 'NONE',  ( -0.7435598031058080482, -3.030962444702889780, 6.932904947974540377 ) ) ;
#9888 = DIRECTION ( 'NONE',  ( -9.349246523159200620E-16, 0.000000000000000000, -1.000000000000000000 ) ) ;
#9889 = CARTESIAN_POINT ( 'NONE',  ( -1.899999999999999911, 4.700000000000000178, 1.600000000000000089 ) ) ;
#9890 = CARTESIAN_POINT ( 'NONE',  ( -0.9002849211310044453, -5.466525423728811006, 7.196465912290821443 ) ) ;
#9891 = ORIENTED_EDGE ( 'NONE', *, *, #10067, .F. ) ;
#9892 = EDGE_LOOP ( 'NONE', ( #9649, #12767, #6599, #15670 ) ) ;
#9893 = CARTESIAN_POINT ( 'NONE',  ( -1.596341326794980198, -5.264406779661019442, 2.970780074643820878 ) ) ;
#9894 = DIRECTION ( 'NONE',  ( 0.000000000000000000, 0.000000000000000000, -1.000000000000000000 ) ) ;
#9895 = LINE ( 'NONE', #14248, #10581 ) ;
#9896 = ORIENTED_EDGE ( 'NONE', *, *, #13790, .F. ) ;
#9897 = B_SPLINE_CURVE_WITH_KNOTS ( 'NONE', 3,
 ( #8281, #9847, #6882, #4952, #13921, #2186, #9302, #1238, #4098, #7829, #792, #5488, #12099, #2280, #8372, #13476, #17719, #15503, #9754, #5051, #6968, #15419, #2725, #16880, #12616, #5591, #6430, #11236, #4188, #3561, #2812, #10704, #16347, #2908, #123, #1520, #5860, #10118, #11506, #17136, #7079, #4275, #8722, #7172, #5771, #10031, #1788, #14367, #392, #5947, #213, #1692, #15690, #12810, #11414, #3000, #9934, #15591, #11678, #8553, #8817, #8641, #11328, #7252, #11586, #308, #1421, #15771, #14468, #1607, #4539, #12723, #8453, #7345, #7432, #14288, #13074, #17302, #6031, #17046, #4630, #12894, #3079, #17217, #10191, #4461, #4370, #12987, #15855, #10290, #3161, #15957, #14200, #14088, #39, #5683, #16965, #16119, #3521, #16039, #13251, #11782, #9167, #7696, #849, #17670, #14922, #17405, #14828, #14630, #570, #4809, #2233, #2141, #13531, #746, #13342, #7786, #10458, #1945, #7600, #13433, #3258, #3417, #6380, #10751, #9066, #14726, #6118, #2041, #12049, #5008, #14548, #10553, #9263, #655, #10662, #1864, #8902, #16307, #7879, #6213, #3613, #3338, #6293, #11870, #6488, #11953, #17567, #4901, #12148, #4725, #17768, #5100, #16214, #7512, #10375, #13157, #8983, #474, #17489, #2434, #12420, #3980, #8162, #12507, #6582, #9459, #2609, #15396, #2514, #3701, #15206, #17949, #16758, #8349, #15021, #5193, #6945, #8259, #2697, #12236, #13898, #17854, #13720, #1034, #18042, #6672 ),
 .UNSPECIFIED., .F., .F.,
 ( 4, 1, 1, 1, 1, 1, 1, 1, 1, 1, 1, 1, 1, 1, 1, 1, 1, 1, 1, 1, 1, 1, 1, 1, 1, 1, 1, 1, 1, 1, 1, 1, 1, 1, 1, 1, 1, 1, 1, 1, 1, 1, 1, 1, 1, 1, 1, 1, 1, 1, 1, 1, 1, 1, 1, 1, 1, 1, 1, 1, 1, 1, 1, 1, 1, 1, 1, 1, 1, 1, 1, 1, 1, 1, 1, 1, 1, 1, 1, 1, 1, 1, 1, 1, 1, 1, 1, 1, 1, 1, 1, 1, 1, 1, 1, 1, 1, 1, 1, 1, 1, 1, 1, 1, 1, 1, 1, 1, 1, 1, 1, 1, 1, 1, 1, 1, 1, 1, 1, 1, 1, 1, 1, 1, 1, 1, 1, 1, 1, 1, 1, 1, 1, 1, 1, 1, 1, 1, 1, 1, 1, 1, 1, 1, 1, 1, 1, 1, 1, 1, 1, 1, 1, 1, 1, 1, 1, 1, 1, 1, 1, 1, 1, 1, 1, 1, 1, 1, 1, 1, 1, 1, 1, 1, 1, 1, 1, 1, 1, 1, 1, 1, 1, 1, 1, 4 ),
 ( 0.7853981633974479459, 0.8787968639095770085, 0.9721955644217059600, 1.065594264933839908, 1.158992965445959866, 1.252391665958090039, 1.345790366470219990, 1.439189066982349940, 1.532587767494480113, 1.625986468006610064, 1.719385168518740015, 1.812783869030869965, 1.906182569543000138, 1.999581270055129867, 2.092979970567249826, 2.186378671079379998, 2.279777371591510171, 2.373176072103639900, 2.466574772615769628, 2.559973473127900245, 2.653372173640029974, 2.746770874152160147, 2.840169574664289875, 2.933568275176409834, 3.026966975688540007, 3.120365676200670180, 3.213764376712799908, 3.307163077224930081, 3.400561777737059810, 3.493960478249190427, 3.587359178761320155, 3.680757879273439670, 3.774156579785570287, 3.867555280297700016, 3.960953980809830188, 4.054352681321960361, 4.147751381834090090, 4.241150082346219818, 4.334548782858350435, 4.427947483370480164, 4.521346183882600123, 4.614744884394729851, 4.708143584906859580, 4.801542285418989309, 4.894940985931119926, 4.988339686443250542, 5.081738386955380271, 5.175137087467510000, 5.268535787979639728, 5.361934488491760575, 5.455333189003890304, 5.548731889516020033, 5.642130590028149761, 5.735529290540279490, 5.828927991052410107, 5.922326691564539836, 6.015725392076670452, 6.109124092588789523, 6.202522793100920140, 6.295921493613049869, 6.389320194125180485, 6.482718894637310214, 6.576117595149439943, 6.669516295661569671, 6.762914996173699400, 6.856313696685830017, 6.949712397197949976, 7.043111097710079704, 7.136509798222209433, 7.229908498734340050, 7.323307199246470667, 7.416705899758600395, 7.510104600270730124, 7.603503300782859853, 7.696902001294989581, 7.790300701807110428, 7.883699402319240157, 7.977098102831369886, 8.070496803343500503, 8.163895503855631119, 8.257294204367759960, 8.350692904879890577, 8.444091605392019417, 8.537490305904137600, 8.630889006416269993, 8.724287706928398833, 8.817686407440529450, 8.911085107952660067, 9.004483808464788908, 9.097882508976921301, 9.191281209489050141, 9.284679910001178982, 9.378078610513298941, 9.471477311025429557, 9.564876011537560174, 9.658274712049690791, 9.751673412561819632, 9.845072113073950248, 9.938470813586080865, 10.03186951409819905, 10.12526821461029947, 10.21866691512249936, 10.31206561563459978, 10.40546431614669842, 10.49886301665890009, 10.59226171717100051, 10.68566041768310093, 10.77905911819519957, 10.87245781870739947, 10.96585651921949989, 11.05925521973160031, 11.15265392024380020, 11.24605262075590062, 11.33945132126800104, 11.43285002178009968, 11.52624872229229958, 11.61964742280439999, 11.71304612331650041, 11.80644482382869853, 11.89984352434079895, 11.99324222485290115, 12.08664092536500156, 12.18003962587719968, 12.27343832638930010, 12.36683702690140052, 12.46023572741360042, 12.55363442792569906, 12.64703312843779948, 12.74043182894989990, 12.83383052946209979, 12.92722922997419843, 13.02062793048630063, 13.11402663099850052, 13.20742533151059916, 13.30082403202269958, 13.39422273253480000, 13.48762143304700167, 13.58102013355910032, 13.67441883407120073, 13.76781753458340063, 13.86121623509549927, 13.95461493560759969, 14.04801363611970011, 14.14141233663190000, 14.23481103714399865, 14.32820973765609907, 14.42160843816829896, 14.51500713868040116, 14.60840583919249980, 14.70180453970460022, 14.79520324021680011, 14.88860194072889875, 14.98200064124100095, 15.07539934175320084, 15.16879804226530126, 15.26219674277739990, 15.35559544328959980, 15.44899414380170022, 15.54239284431380064, 15.63579154482589928, 15.72919024533809740, 15.82258894585020137, 15.91598764636230001, 16.00938634687449991, 16.10278504738660033, 16.19618374789870074, 16.28958244841080116, 16.38298114892299751, 16.47637984943510148, 16.56977854994720545, 16.66317725045940179, 16.75657595097149866, 16.84997465148359908, 16.94337335199570305, 17.03677205250789939, 17.13017075301999981, 17.22356945353210023, 17.31696815404430012, 17.41036685455640054, 17.50376555506850096, 17.59716425558059782, 17.69056295609280127, 17.78396165660489814, 17.87736035711699856, 17.97075905762920200, 18.06415775814129887 ),
 .UNSPECIFIED. ) ;
#9898 = CARTESIAN_POINT ( 'NONE',  ( 2.316126390218360420, -0.8651516338920848259, 3.404364157709320438 ) ) ;
#9899 = CARTESIAN_POINT ( 'NONE',  ( -4.404543739248539922E-17, 5.113553479078069230, 6.680683419527140288 ) ) ;
#9900 = CARTESIAN_POINT ( 'NONE',  ( 0.2735655355027601376, -5.004947479095214646, 2.050775599341920330 ) ) ;
#9901 = CARTESIAN_POINT ( 'NONE',  ( -0.1749999999999999889, 9.099999999999999645, 0.5999999999999999778 ) ) ;
#9902 = CARTESIAN_POINT ( 'NONE',  ( -2.353452300571019506, -1.474488005747550012, 4.697179287168410156 ) ) ;
#9903 = DIRECTION ( 'NONE',  ( 0.000000000000000000, -1.000000000000000000, 0.000000000000000000 ) ) ;
#9904 = CARTESIAN_POINT ( 'NONE',  ( 1.869848057046569867, -4.288530012270459935, 6.129130480762009725 ) ) ;
#9905 = FACE_OUTER_BOUND ( 'NONE', #15733, .T. ) ;
#9906 = CARTESIAN_POINT ( 'NONE',  ( 1.181710496343130190, -2.798079561820010941, 6.378827610405712001 ) ) ;
#9907 = DIRECTION ( 'NONE',  ( 1.000000000000000000, 2.337311630789800155E-16, 2.220446049250309876E-16 ) ) ;
#9908 = DIRECTION ( 'NONE',  ( 1.233581138472399909E-16, 6.167905692361979821E-17, -1.000000000000000000 ) ) ;
#9909 = VERTEX_POINT ( 'NONE', #14982 ) ;
#9910 = CARTESIAN_POINT ( 'NONE',  ( 0.009452110982654814836, -0.3001920447045380858, 2.649999999999998579 ) ) ;
#9911 = ORIENTED_EDGE ( 'NONE', *, *, #6353, .T. ) ;
#9912 = DIRECTION ( 'NONE',  ( 1.224646799147350002E-16, -1.000000000000000000, -6.123233995736759873E-17 ) ) ;
#9913 = ORIENTED_EDGE ( 'NONE', *, *, #13766, .T. ) ;
#9914 = DIRECTION ( 'NONE',  ( 1.000000000000000000, 0.000000000000000000, 1.305527901448219810E-16 ) ) ;
#9915 = VERTEX_POINT ( 'NONE', #6632 ) ;
#9916 = CARTESIAN_POINT ( 'NONE',  ( -1.202278654260740876, -5.179872881355935377, 6.364093491318035589 ) ) ;
#9917 = CARTESIAN_POINT ( 'NONE',  ( 1.800000000000000044, 0.5999999999999999778, 1.600000000000000089 ) ) ;
#9918 = LINE ( 'NONE', #11120, #9057 ) ;
#9919 = FACE_OUTER_BOUND ( 'NONE', #17880, .T. ) ;
#9920 = LINE ( 'NONE', #16952, #6065 ) ;
#9921 = FACE_OUTER_BOUND ( 'NONE', #3001, .T. ) ;
#9922 = CARTESIAN_POINT ( 'NONE',  ( 2.500000000000000000, 0.8000000000000000444, -1.776356839400249676E-15 ) ) ;
#9923 = CARTESIAN_POINT ( 'NONE',  ( 0.2365712905368450025, -2.192584066324519743, 2.358466376073659720 ) ) ;
#9924 = CARTESIAN_POINT ( 'NONE',  ( -0.9361665894546699063, -3.314262780522333696, 2.872845392579789880 ) ) ;
#9925 = AXIS2_PLACEMENT_3D ( 'NONE', #15409, #7070, #2894 ) ;
#9926 = ADVANCED_FACE ( 'NONE', ( #14782 ), #621, .F. ) ;
#9927 = CARTESIAN_POINT ( 'NONE',  ( 1.489797906646480596, -0.1112288135593229726, 6.112509577910826941 ) ) ;
#9928 = CARTESIAN_POINT ( 'NONE',  ( -5.204748896376247618E-17, 7.250000000000000000, 6.299999999999999822 ) ) ;
#9929 = ADVANCED_FACE ( 'NONE', ( #16554 ), #5153, .T. ) ;
#9930 = EDGE_CURVE ( 'NONE', #12188, #14967, #3760, .T. ) ;
#9931 = FACE_OUTER_BOUND ( 'NONE', #832, .T. ) ;
#9932 = CARTESIAN_POINT ( 'NONE',  ( 2.287919158821199783, -1.051457940198389895, 5.251517552016890633 ) ) ;
#9933 = VERTEX_POINT ( 'NONE', #16894 ) ;
#9934 = CARTESIAN_POINT ( 'NONE',  ( -0.8429265834919730249, -2.076142624883080323, 2.502678798553459760 ) ) ;
#9935 = ORIENTED_EDGE ( 'NONE', *, *, #2064, .F. ) ;
#9936 = ORIENTED_EDGE ( 'NONE', *, *, #1840, .T. ) ;
#9937 = CARTESIAN_POINT ( 'NONE',  ( 1.917298190932609003, -2.103271789531340641, 3.335187436117900805 ) ) ;
#9938 = CARTESIAN_POINT ( 'NONE',  ( 0.000000000000000000, 0.000000000000000000, 0.000000000000000000 ) ) ;
#9939 = CARTESIAN_POINT ( 'NONE',  ( 1.467041701146838406, -5.422033898305085309, 6.911479965439912831 ) ) ;
#9940 = TOROIDAL_SURFACE ( 'NONE', #3411, 0.2999999999999999889, 0.2500000000000000000 ) ;
#9941 = ORIENTED_EDGE ( 'NONE', *, *, #13069, .F. ) ;
#9942 = CARTESIAN_POINT ( 'NONE',  ( 2.500000000000000000, 2.799999999999999822, 0.6099999999999999867 ) ) ;
#9943 = CARTESIAN_POINT ( 'NONE',  ( -1.994315313497099229, -0.5135593220338985354, 5.187224322759965922 ) ) ;
#9944 = ORIENTED_EDGE ( 'NONE', *, *, #6476, .F. ) ;
#9945 = ADVANCED_FACE ( 'NONE', ( #6808 ), #14019, .T. ) ;
#9946 = CARTESIAN_POINT ( 'NONE',  ( 2.500000000000000000, 10.00000000000000000, -1.206091987257470116E-15 ) ) ;
#9947 = SPHERICAL_SURFACE ( 'NONE', #11467, 0.4166666666666670182 ) ;
#9948 = DIRECTION ( 'NONE',  ( 1.000000000000000000, 0.000000000000000000, 0.000000000000000000 ) ) ;
#9949 = CARTESIAN_POINT ( 'NONE',  ( 1.712910428781929006, -2.704926408666860738, 5.831741890007691609 ) ) ;
#9951 = ADVANCED_FACE ( 'NONE', ( #6894 ), #10977, .T. ) ;
#9950 = LINE ( 'NONE', #12633, #16478 ) ;
#9952 = VERTEX_POINT ( 'NONE', #15519 ) ;
#9953 = DIRECTION ( 'NONE',  ( 1.739311637268509859E-16, 6.049014748177290126E-16, -1.000000000000000000 ) ) ;
#9954 = FACE_OUTER_BOUND ( 'NONE', #290, .T. ) ;
#9955 = EDGE_CURVE ( 'NONE', #5117, #6801, #2540, .T. ) ;
#9956 = FACE_OUTER_BOUND ( 'NONE', #15448, .T. ) ;
#9957 = CIRCLE ( 'NONE', #4325, 0.1999999999999999833 ) ;
#9958 = ORIENTED_EDGE ( 'NONE', *, *, #17600, .T. ) ;
#9959 = CARTESIAN_POINT ( 'NONE',  ( 6.429395695523600208E-16, 3.500000000000000000, 5.100000000000000533 ) ) ;
#9960 = CARTESIAN_POINT ( 'NONE',  ( -1.364983921886200546, -4.865515740159335856, 2.403349116468209257 ) ) ;
#9961 = CARTESIAN_POINT ( 'NONE',  ( -0.5137283630188880235, -5.462076271186444565, 6.687652957477222770 ) ) ;
#9962 = ORIENTED_EDGE ( 'NONE', *, *, #9137, .F. ) ;
#9963 = CARTESIAN_POINT ( 'NONE',  ( 2.340070819011249803, -0.08008474576271228107, 4.950151441910538352 ) ) ;
#9964 = CARTESIAN_POINT ( 'NONE',  ( 1.300961508564179914, -5.422033898305079092, 6.661123742937279602 ) ) ;
#9965 = CYLINDRICAL_SURFACE ( 'NONE', #9662, 0.6100000000000000977 ) ;
#9966 = AXIS2_PLACEMENT_3D ( 'NONE', #1121, #9545, #8254 ) ;
#9967 = EDGE_LOOP ( 'NONE', ( #14086, #13376, #14181, #13635 ) ) ;
#9968 = CARTESIAN_POINT ( 'NONE',  ( 0.5000000000000000000, 3.500000000000000000, 6.100000000000000533 ) ) ;
#9969 = CIRCLE ( 'NONE', #14720, 0.01000000000000002623 ) ;
#9970 = CARTESIAN_POINT ( 'NONE',  ( -1.869848057046539891, -1.311469987729539932, 6.129130480762059463 ) ) ;
#9971 = VECTOR ( 'NONE', #15177, 1000.000000000000000 ) ;
#9972 = CARTESIAN_POINT ( 'NONE',  ( 2.350000000000000089, -5.599999999999999645, 6.400000000000000355 ) ) ;
#9973 = PRESENTATION_LAYER_ASSIGNMENT (  '', '', ( #9672 ) ) ;
#9974 = CARTESIAN_POINT ( 'NONE',  ( -2.048006021857541548, -3.058091609351150986, 4.556566471620694614 ) ) ;
#9976 = EDGE_CURVE ( 'NONE', #851, #2878, #8192, .T. ) ;
#9975 = LINE ( 'NONE', #4222, #10539 ) ;
#9977 = ORIENTED_EDGE ( 'NONE', *, *, #18053, .T. ) ;
#9978 = VECTOR ( 'NONE', #9417, 1000.000000000000000 ) ;
#9979 = CARTESIAN_POINT ( 'NONE',  ( 1.733739193136930146, -5.074965191738780135, 2.966260806863060040 ) ) ;
#9980 = CARTESIAN_POINT ( 'NONE',  ( 0.4917262214558945632, -0.008898305084746043966, 2.092115739186370948 ) ) ;
#9981 = LINE ( 'NONE', #16919, #2166 ) ;
#9982 = EDGE_CURVE ( 'NONE', #10479, #1710, #5500, .T. ) ;
#9983 = CARTESIAN_POINT ( 'NONE',  ( 1.000000000000000000, 5.400000000000000355, 7.700000000000000178 ) ) ;
#9984 = CARTESIAN_POINT ( 'NONE',  ( 1.661700935788380074, -5.037500000000000533, 3.038299064211610112 ) ) ;
#9985 = VERTEX_POINT ( 'NONE', #18071 ) ;
#9986 = CIRCLE ( 'NONE', #1973, 0.5000000000000000000 ) ;
#9987 = ORIENTED_EDGE ( 'NONE', *, *, #14723, .T. ) ;
#9988 = CARTESIAN_POINT ( 'NONE',  ( -2.011500846714318502, -5.251059322033899690, 3.478373409938471550 ) ) ;
#9989 = CARTESIAN_POINT ( 'NONE',  ( 0.1749999999999999889, 9.299999999999998934, 1.600000000000000089 ) ) ;
#9990 = ORIENTED_EDGE ( 'NONE', *, *, #11714, .F. ) ;
#9991 = VECTOR ( 'NONE', #8356, 1000.000000000000000 ) ;
#9992 = CARTESIAN_POINT ( 'NONE',  ( -2.296954468777729463, -4.963890372630819670, 4.187412587068699565 ) ) ;
#9993 = AXIS2_PLACEMENT_3D ( 'NONE', #1658, #281, #10166 ) ;
#9994 =( NAMED_UNIT ( * ) SI_UNIT ( $, .STERADIAN. ) SOLID_ANGLE_UNIT ( ) );
#9995 = CARTESIAN_POINT ( 'NONE',  ( 1.732245706108171746, -5.033893599512585304, 2.684512698446369861 ) ) ;
#9996 = CARTESIAN_POINT ( 'NONE',  ( 1.630481553867769939, -2.056695212954759988, 3.002862530617850023 ) ) ;
#9998 = EDGE_CURVE ( 'NONE', #12787, #10006, #4127, .T. ) ;
#9997 = LINE ( 'NONE', #7043, #10854 ) ;
#9999 = VECTOR ( 'NONE', #5245, 1000.000000000000000 ) ;
#10000 = CARTESIAN_POINT ( 'NONE',  ( 0.6096110657044089276, -3.799475958216410376, 2.426869991387509806 ) ) ;
#10001 = DIRECTION ( 'NONE',  ( -1.000000000000000000, 0.000000000000000000, 0.000000000000000000 ) ) ;
#10002 = CARTESIAN_POINT ( 'NONE',  ( 1.909909196654749897, -4.032358841099289215, 3.946907241329673521 ) ) ;
#10003 = CARTESIAN_POINT ( 'NONE',  ( -2.500000000000000000, 11.25000000000000000, 7.649999999999999467 ) ) ;
#10004 = CIRCLE ( 'NONE', #7927, 0.5500000000000001554 ) ;
#10005 = ORIENTED_EDGE ( 'NONE', *, *, #16944, .T. ) ;
#10006 = VERTEX_POINT ( 'NONE', #3926 ) ;
#10007 = AXIS2_PLACEMENT_3D ( 'NONE', #2772, #166, #4323 ) ;
#10008 = EDGE_CURVE ( 'NONE', #17362, #2860, #9770, .T. ) ;
#10009 = CARTESIAN_POINT ( 'NONE',  ( 2.500000000000000000, 1.148961478048660025E-16, 3.600000000000000089 ) ) ;
#10010 = FACE_OUTER_BOUND ( 'NONE', #5054, .T. ) ;
#10011 = ORIENTED_EDGE ( 'NONE', *, *, #4924, .T. ) ;
#10012 = LINE ( 'NONE', #15483, #16805 ) ;
#10013 = VECTOR ( 'NONE', #11316, 1000.000000000000000 ) ;
#10014 = VECTOR ( 'NONE', #17409, 1000.000000000000000 ) ;
#10015 = ORIENTED_EDGE ( 'NONE', *, *, #8669, .T. ) ;
#10016 = CARTESIAN_POINT ( 'NONE',  ( -3.421358338620380043E-15, -5.299999999999999822, 2.350000000000000089 ) ) ;
#10017 = CARTESIAN_POINT ( 'NONE',  ( -2.500000000000000000, 8.500000000000000000, 0.6099999999999999867 ) ) ;
#10018 = DIRECTION ( 'NONE',  ( -1.000000000000000000, 0.000000000000000000, 0.000000000000000000 ) ) ;
#10019 = AXIS2_PLACEMENT_3D ( 'NONE', #15181, #3773, #17639 ) ;
#10020 = VECTOR ( 'NONE', #927, 1000.000000000000114 ) ;
#10021 = CARTESIAN_POINT ( 'NONE',  ( 1.983927814618709873E-15, 10.80000000000000071, 8.599999999999999645 ) ) ;
#10022 = LINE ( 'NONE', #12975, #10871 ) ;
#10023 = LINE ( 'NONE', #17035, #2345 ) ;
#10024 = CARTESIAN_POINT ( 'NONE',  ( 0.8748826269292639957, -2.262448931189380286, 2.515205712983200392 ) ) ;
#10025 = CARTESIAN_POINT ( 'NONE',  ( 1.842787987253230897, -3.710163681423226389, 3.794994874786191907 ) ) ;
#10026 = CARTESIAN_POINT ( 'NONE',  ( 1.549742865090599997, -0.4156779661016959948, 6.471102547561449647 ) ) ;
#10027 = CARTESIAN_POINT ( 'NONE',  ( -1.899999999999999911, 0.5999999999999999778, 6.599999999999999645 ) ) ;
#10028 = DIRECTION ( 'NONE',  ( -1.000000000000000000, 0.000000000000000000, 0.000000000000000000 ) ) ;
#10029 = VERTEX_POINT ( 'NONE', #15611 ) ;
#10030 = CARTESIAN_POINT ( 'NONE',  ( 1.088937603231269646, -0.02669491525423760975, 2.959627624143540192 ) ) ;
#10031 = CARTESIAN_POINT ( 'NONE',  ( -2.316639661709700260, -1.819971453711900056, 4.285359956977770501 ) ) ;
#10032 = ORIENTED_EDGE ( 'NONE', *, *, #8470, .T. ) ;
#10033 = CIRCLE ( 'NONE', #17109, 0.6500000000000003553 ) ;
#10034 = CARTESIAN_POINT ( 'NONE',  ( -1.899999999999999911, 2.799999999999999822, 1.600000000000000089 ) ) ;
#10035 = ORIENTED_EDGE ( 'NONE', *, *, #3473, .T. ) ;
#10036 = CARTESIAN_POINT ( 'NONE',  ( 0.6343239990445398435, -3.500569086828631438, 2.433641963034071765 ) ) ;
#10037 = PRODUCT_CONTEXT ( 'NONE', #13728, 'mechanical' ) ;
#10038 = CARTESIAN_POINT ( 'NONE',  ( -2.386628511786350160, -5.546610169491530407, 3.539457309197792778 ) ) ;
#10039 = ORIENTED_EDGE ( 'NONE', *, *, #16756, .T. ) ;
#10040 = CARTESIAN_POINT ( 'NONE',  ( -1.630481553867809907, -3.543304787045240101, 3.002862530617889547 ) ) ;
#10041 = ADVANCED_FACE ( 'NONE', ( #16703 ), #15433, .F. ) ;
#10042 = CARTESIAN_POINT ( 'NONE',  ( -0.7982439214406890082, -0.4690677966101705065, 6.591424794228156081 ) ) ;
#10043 = VERTEX_POINT ( 'NONE', #15238 ) ;
#10044 = FACE_OUTER_BOUND ( 'NONE', #3102, .T. ) ;
#10045 = CARTESIAN_POINT ( 'NONE',  ( -0.5500000000000000444, 3.050000000000000266, 3.299999999999999822 ) ) ;
#10046 = VECTOR ( 'NONE', #3892, 1000.000000000000000 ) ;
#10047 = CARTESIAN_POINT ( 'NONE',  ( -1.642659730162759901, -1.936412895153350133, 3.468508687188699646 ) ) ;
#10048 = CARTESIAN_POINT ( 'NONE',  ( 1.899999999999999911, 0.5999999999999999778, 1.600000000000000089 ) ) ;
#10049 = ORIENTED_EDGE ( 'NONE', *, *, #5746, .T. ) ;
#10050 = PLANE ( 'NONE',  #16480 ) ;
#10051 = EDGE_CURVE ( 'NONE', #6712, #229, #7095, .T. ) ;
#10052 = ORIENTED_EDGE ( 'NONE', *, *, #15933, .F. ) ;
#10053 = CARTESIAN_POINT ( 'NONE',  ( -1.899999999999999911, 0.7500000000000000000, 7.649999999999999467 ) ) ;
#10054 = CARTESIAN_POINT ( 'NONE',  ( 2.234315482767910144, -5.359745762711869865, 3.960850823455320580 ) ) ;
#10055 = EDGE_CURVE ( 'NONE', #9144, #14593, #18002, .T. ) ;
#10056 = CARTESIAN_POINT ( 'NONE',  ( -2.143090896833109493, -0.2046610169491529518, 5.672454929438351279 ) ) ;
#10057 = AXIS2_PLACEMENT_3D ( 'NONE', #12215, #7854, #10728 ) ;
#10058 = DIRECTION ( 'NONE',  ( 1.000000000000000000, 0.000000000000000000, 0.000000000000000000 ) ) ;
#10059 = ADVANCED_FACE ( 'NONE', ( #4201 ), #9861, .T. ) ;
#10060 = ADVANCED_FACE ( 'NONE', ( #7094 ), #5698, .F. ) ;
#10061 = ORIENTED_EDGE ( 'NONE', *, *, #3226, .F. ) ;
#10062 = CARTESIAN_POINT ( 'NONE',  ( 0.7500000000000000000, 3.050000000000000266, 2.699264068711930253 ) ) ;
#10063 = ADVANCED_FACE ( 'NONE', ( #5588 ), #1516, .T. ) ;
#10064 = CARTESIAN_POINT ( 'NONE',  ( -2.262450597846770162, -1.404623140882689913, 5.348122657979730299 ) ) ;
#10065 = EDGE_CURVE ( 'NONE', #7652, #13315, #7249, .T. ) ;
#10066 = DIRECTION ( 'NONE',  ( -2.337311630789800155E-16, 1.000000000000000000, 0.000000000000000000 ) ) ;
#10067 = EDGE_CURVE ( 'NONE', #7791, #5801, #16241, .T. ) ;
#10068 = CARTESIAN_POINT ( 'NONE',  ( 1.798783563193339985, -2.382731248990799244, 5.689585537188965425 ) ) ;
#10069 = CARTESIAN_POINT ( 'NONE',  ( 1.850000000000000089, 11.25000000000000000, 7.649999999999999467 ) ) ;
#10070 = ORIENTED_EDGE ( 'NONE', *, *, #6236, .T. ) ;
#10071 = AXIS2_PLACEMENT_3D ( 'NONE', #2187, #13583, #16163 ) ;
#10072 = LINE ( 'NONE', #4762, #1441 ) ;
#10073 = CARTESIAN_POINT ( 'NONE',  ( -1.943632316591239917, -0.5536016949152539057, 3.373048379518170048 ) ) ;
#10074 = CARTESIAN_POINT ( 'NONE',  ( -0.7998959936908373036, -0.4646186440677965712, 7.230419212249866945 ) ) ;
#10075 = CARTESIAN_POINT ( 'NONE',  ( 0.8242394280877100021, -4.428259742000189902, 6.904399023015010073 ) ) ;
#10076 = CARTESIAN_POINT ( 'NONE',  ( -1.599999999999880185, 11.40000000000000036, -2.399999999999999911 ) ) ;
#10077 = PLANE ( 'NONE',  #3850 ) ;
#10078 = CARTESIAN_POINT ( 'NONE',  ( 2.293398556041700065, -5.064194915254240037, 4.171956209133470317 ) ) ;
#10079 = ORIENTED_EDGE ( 'NONE', *, *, #2622, .F. ) ;
#10080 = ORIENTED_EDGE ( 'NONE', *, *, #13112, .T. ) ;
#10081 = LINE ( 'NONE', #14153, #13035 ) ;
#10082 = CARTESIAN_POINT ( 'NONE',  ( -0.6914213562373099364, 6.450000000000000178, 2.557842712474620139 ) ) ;
#10083 = ADVANCED_FACE ( 'NONE', ( #15156 ), #2722, .F. ) ;
#10084 = ORIENTED_EDGE ( 'NONE', *, *, #682, .F. ) ;
#10085 = AXIS2_PLACEMENT_3D ( 'NONE', #9680, #1174, #4213 ) ;
#10086 = CARTESIAN_POINT ( 'NONE',  ( 2.306572132003631648, -1.121322805063259542, 6.012569500204132389 ) ) ;
#10087 = CARTESIAN_POINT ( 'NONE',  ( 1.307725206348619995, -0.7471169921413569615, 2.732408283416570161 ) ) ;
#10088 = LINE ( 'NONE', #7400, #7606 ) ;
#10089 = CARTESIAN_POINT ( 'NONE',  ( 2.237394498046680003, -2.336154672414219924, 5.429939413646329704 ) ) ;
#10090 = CARTESIAN_POINT ( 'NONE',  ( -0.3367924244280810497, 2.254758922476410188, 8.300000000000000711 ) ) ;
#10091 = CARTESIAN_POINT ( 'NONE',  ( 1.571912189623089873, -4.335106588847041031, 6.451524409078630562 ) ) ;
#10092 = DIRECTION ( 'NONE',  ( 0.000000000000000000, 0.000000000000000000, -1.000000000000000000 ) ) ;
#10093 = CARTESIAN_POINT ( 'NONE',  ( -0.03076623656502111559, -4.521412895153344103, 6.752792069673816400 ) ) ;
#10094 = ADVANCED_FACE ( 'NONE', ( #9931 ), #7169, .T. ) ;
#10095 = CARTESIAN_POINT ( 'NONE',  ( -1.641808337277740115, -0.4868644067796619734, 6.386111670537629514 ) ) ;
#10096 = LINE ( 'NONE', #15746, #1428 ) ;
#10097 = DIRECTION ( 'NONE',  ( 0.000000000000000000, 0.000000000000000000, 1.000000000000000000 ) ) ;
#10098 = ORIENTED_EDGE ( 'NONE', *, *, #13830, .F. ) ;
#10099 = FACE_OUTER_BOUND ( 'NONE', #7179, .T. ) ;
#10100 = ORIENTED_EDGE ( 'NONE', *, *, #4570, .T. ) ;
#10101 = FACE_OUTER_BOUND ( 'NONE', #3133, .T. ) ;
#10102 = EDGE_CURVE ( 'NONE', #15567, #5243, #17133, .T. ) ;
#10103 = ORIENTED_EDGE ( 'NONE', *, *, #6297, .T. ) ;
#10104 = CARTESIAN_POINT ( 'NONE',  ( 1.869504824896970119, -5.395338983050850246, 5.548311746956850143 ) ) ;
#10105 = CARTESIAN_POINT ( 'NONE',  ( 2.121170185508189476, -3.663587104846653730, 3.105085978143951486 ) ) ;
#10106 = DIRECTION ( 'NONE',  ( 3.018987445473099952E-48, 1.000000000000000000, 2.465190328815659976E-32 ) ) ;
#10107 = LINE ( 'NONE', #462, #6104 ) ;
#10108 = CARTESIAN_POINT ( 'NONE',  ( -1.485788269501200132, -4.829629811528119099, 2.863981322975839738 ) ) ;
#10109 = CARTESIAN_POINT ( 'NONE',  ( 0.9000000000000000222, 6.450000000000000178, 1.600000000000000089 ) ) ;
#10110 = LINE ( 'NONE', #3069, #11205 ) ;
#10111 = CARTESIAN_POINT ( 'NONE',  ( 1.832842064134690085, -2.728214696955149954, 6.176291182464479945 ) ) ;
#10112 = CARTESIAN_POINT ( 'NONE',  ( -1.764143222953850065, -3.174533050792599731, 3.649904513135073802 ) ) ;
#10113 = CARTESIAN_POINT ( 'NONE',  ( 2.041338374031088865, -0.08008474576271226719, 4.918217215283659627 ) ) ;
#10114 = CARTESIAN_POINT ( 'NONE',  ( -0.1749999999999999889, 5.200000000000000178, 0.5999999999999999778 ) ) ;
#10115 = EDGE_LOOP ( 'NONE', ( #10730, #16198, #18122, #3421, #17010, #2964, #15461, #3781, #6396, #72, #7091, #3702, #9083, #7717, #18061, #12478, #9944, #2239, #8998, #17076, #3907, #17618, #7614, #5096, #8668, #1387, #1248, #10201 ) ) ;
#10116 = CARTESIAN_POINT ( 'NONE',  ( -1.630703155447540631, -3.267686203945749490, 2.606218513833090000 ) ) ;
#10117 = CARTESIAN_POINT ( 'NONE',  ( -1.811729841638700211, -0.2580508474576269640, 3.197954009834299782 ) ) ;
#10118 = CARTESIAN_POINT ( 'NONE',  ( -1.981271652668300298, -1.633665147405599871, 5.970160748022450115 ) ) ;
#10119 = ORIENTED_EDGE ( 'NONE', *, *, #9043, .T. ) ;
#10120 = EDGE_LOOP ( 'NONE', ( #478, #4631, #9941, #8299 ) ) ;
#10121 = CARTESIAN_POINT ( 'NONE',  ( 1.417709711196429412, -3.593722239981790523, 2.821478011237760430 ) ) ;
#10122 = DIRECTION ( 'NONE',  ( 1.000000000000000000, 0.000000000000000000, 0.000000000000000000 ) ) ;
#10123 = CARTESIAN_POINT ( 'NONE',  ( 2.508228811380011081, -5.090889830508485758, 5.566973598334535644 ) ) ;
#10124 = ORIENTED_EDGE ( 'NONE', *, *, #10322, .T. ) ;
#10125 = CARTESIAN_POINT ( 'NONE',  ( -2.050059171113549183, -0.5224576271186435195, 4.809263467226075228 ) ) ;
#10126 = ORIENTED_EDGE ( 'NONE', *, *, #1476, .F. ) ;
#10127 = FACE_OUTER_BOUND ( 'NONE', #7026, .T. ) ;
#10128 = CARTESIAN_POINT ( 'NONE',  ( 2.039016451601951108, -2.588484967225421762, 4.939402908764060740 ) ) ;
#10129 = CARTESIAN_POINT ( 'NONE',  ( 1.250000000000000000, 0.5999999999999999778, 6.100000000000000533 ) ) ;
#10130 = VERTEX_POINT ( 'NONE', #4457 ) ;
#10131 = FACE_OUTER_BOUND ( 'NONE', #14198, .T. ) ;
#10132 = ORIENTED_EDGE ( 'NONE', *, *, #15426, .F. ) ;
#10133 = CARTESIAN_POINT ( 'NONE',  ( 0.1749999999999999889, 4.299999999999999822, 1.600000000000000089 ) ) ;
#10134 = CARTESIAN_POINT ( 'NONE',  ( -1.614765845140348821, -5.493220338983046069, 5.967758800287426446 ) ) ;
#10135 = CARTESIAN_POINT ( 'NONE',  ( -0.1749999999999999889, 4.299999999999999822, 0.5999999999999999778 ) ) ;
#10136 = AXIS2_PLACEMENT_3D ( 'NONE', #2649, #1254, #8475 ) ;
#10137 = DIRECTION ( 'NONE',  ( 4.794417550286630491E-31, -1.000000000000000000, -1.774290917998389804E-45 ) ) ;
#10138 = VERTEX_POINT ( 'NONE', #12613 ) ;
#10139 = PLANE ( 'NONE',  #13804 ) ;
#10140 = CARTESIAN_POINT ( 'NONE',  ( -1.214457691476030110, -1.730659176918720066, 2.684103622926369948 ) ) ;
#10141 = DIRECTION ( 'NONE',  ( -0.7071067811865480168, 0.000000000000000000, 0.7071067811865470176 ) ) ;
#10142 = CARTESIAN_POINT ( 'NONE',  ( -1.181710496343089556, -2.801920438179980710, 6.378827610405741311 ) ) ;
#10143 = CARTESIAN_POINT ( 'NONE',  ( 0.5999999999999999778, 0.5999999999999999778, 7.599999999999999645 ) ) ;
#10144 = ADVANCED_FACE ( 'NONE', ( #12719 ), #36, .F. ) ;
#10145 = VERTEX_POINT ( 'NONE', #17043 ) ;
#10146 = EDGE_CURVE ( 'NONE', #13575, #3076, #291, .T. ) ;
#10147 = DIRECTION ( 'NONE',  ( -1.531342102931250010E-16, 1.000000000000000000, 0.000000000000000000 ) ) ;
#10148 = CARTESIAN_POINT ( 'NONE',  ( -2.043014502273419186, -0.5580508474576266753, 3.006203457898251052 ) ) ;
#10149 = EDGE_CURVE ( 'NONE', #14423, #11652, #4185, .T. ) ;
#10150 = CARTESIAN_POINT ( 'NONE',  ( 2.262450597846779932, -4.195376859117310175, 5.348122657979680561 ) ) ;
#10151 = PLANE ( 'NONE',  #5122 ) ;
#10152 = ADVANCED_FACE ( 'NONE', ( #15499 ), #14085, .T. ) ;
#10153 = CARTESIAN_POINT ( 'NONE',  ( 0.1749999999999999889, 8.500000000000000000, -3.200000000000000178 ) ) ;
#10154 = CARTESIAN_POINT ( 'NONE',  ( -0.1765068388402301069, -5.153177966101685215, 7.347961541693647902 ) ) ;
#10155 = ORIENTED_EDGE ( 'NONE', *, *, #4749, .T. ) ;
#10156 = ORIENTED_EDGE ( 'NONE', *, *, #13815, .T. ) ;
#10157 = CARTESIAN_POINT ( 'NONE',  ( 0.1749999999999999889, 7.700000000000000178, 0.5999999999999999778 ) ) ;
#10158 = FACE_OUTER_BOUND ( 'NONE', #14245, .T. ) ;
#10159 = ORIENTED_EDGE ( 'NONE', *, *, #17493, .F. ) ;
#10160 = DIRECTION ( 'NONE',  ( 0.000000000000000000, 1.000000000000000000, 0.000000000000000000 ) ) ;
#10161 = DIRECTION ( 'NONE',  ( 8.971499188890150495E-16, 0.000000000000000000, 1.000000000000000000 ) ) ;
#10162 = CARTESIAN_POINT ( 'NONE',  ( 0.2620510901103109691, -1.893677194936739916, 2.361180871966390260 ) ) ;
#10163 = CARTESIAN_POINT ( 'NONE',  ( -0.009452110982655139229, -5.299807955295460005, 2.350000000000000089 ) ) ;
#10164 = CARTESIAN_POINT ( 'NONE',  ( 1.668426559427239608, -1.214475958216409746, 6.763847501342977075 ) ) ;
#10165 = LINE ( 'NONE', #14062, #14652 ) ;
#10166 = DIRECTION ( 'NONE',  ( 1.224646799147349016E-16, 0.000000000000000000, 1.000000000000000000 ) ) ;
#10167 = CARTESIAN_POINT ( 'NONE',  ( -1.934380261529029754, -4.824160642901089702, 5.387804366397155320 ) ) ;
#10168 = EDGE_CURVE ( 'NONE', #15958, #1792, #2904, .T. ) ;
#10169 = CYLINDRICAL_SURFACE ( 'NONE', #10891, 0.3500000000000001998 ) ;
#10170 = DIRECTION ( 'NONE',  ( 0.000000000000000000, -1.000000000000000000, 2.493473113004670213E-16 ) ) ;
#10171 = ORIENTED_EDGE ( 'NONE', *, *, #1618, .F. ) ;
#10172 = VERTEX_POINT ( 'NONE', #1416 ) ;
#10173 = DIRECTION ( 'NONE',  ( -1.000000000000000000, -1.908195823574489776E-16, -1.110223024625159992E-16 ) ) ;
#10174 = DIRECTION ( 'NONE',  ( -1.305527901448219810E-16, 6.123233995736909017E-17, 1.000000000000000000 ) ) ;
#10175 = ORIENTED_EDGE ( 'NONE', *, *, #15217, .T. ) ;
#10176 = CARTESIAN_POINT ( 'NONE',  ( -0.1910247150515231307, -5.295550847457634269, 2.655937705488500722 ) ) ;
#10177 = DIRECTION ( 'NONE',  ( 0.000000000000000000, 0.000000000000000000, 1.000000000000000000 ) ) ;
#10178 = CARTESIAN_POINT ( 'NONE',  ( 1.700860513939579599, -2.475884402143949892, 6.737200825918507441 ) ) ;
#10179 = CARTESIAN_POINT ( 'NONE',  ( -1.899999999999999911, 2.799999999999999822, 0.6099999999999999867 ) ) ;
#10180 = FACE_OUTER_BOUND ( 'NONE', #17809, .T. ) ;
#10181 = CARTESIAN_POINT ( 'NONE',  ( 0.3042893218813439438, 6.450000000000000178, 2.170710678118660031 ) ) ;
#10182 = DIRECTION ( 'NONE',  ( 1.000000000000000000, 0.000000000000000000, 0.000000000000000000 ) ) ;
#10183 = CARTESIAN_POINT ( 'NONE',  ( -0.7435598031058080482, -3.030962444702889780, 6.932904947974540377 ) ) ;
#10184 = CARTESIAN_POINT ( 'NONE',  ( 0.3257255101953561716, -4.175929447188994281, 6.727018681373227338 ) ) ;
#10185 = EDGE_CURVE ( 'NONE', #12466, #14118, #18236, .T. ) ;
#10186 = CARTESIAN_POINT ( 'NONE',  ( 0.5999999999999999778, 0.5999999999999999778, 7.599999999999999645 ) ) ;
#10187 = CARTESIAN_POINT ( 'NONE',  ( 1.399999999999999911, -7.000000000000000000, 6.100000000000000533 ) ) ;
#10188 = ORIENTED_EDGE ( 'NONE', *, *, #14675, .T. ) ;
#10189 = CARTESIAN_POINT ( 'NONE',  ( -0.8001094918299070935, -4.292370888630430592, 7.230402832373842514 ) ) ;
#10190 = CARTESIAN_POINT ( 'NONE',  ( 1.489797906646480596, -0.1112288135593229726, 6.112509577910826941 ) ) ;
#10191 = CARTESIAN_POINT ( 'NONE',  ( 1.832842064134690085, -2.728214696955149954, 6.176291182464479945 ) ) ;
#10192 = VERTEX_POINT ( 'NONE', #2809 ) ;
#10193 = CARTESIAN_POINT ( 'NONE',  ( 2.500000000000000000, 2.799999999999999822, 0.5999999999999999778 ) ) ;
#10194 = ORIENTED_EDGE ( 'NONE', *, *, #13329, .F. ) ;
#10195 = CARTESIAN_POINT ( 'NONE',  ( 1.881914957835459701, -3.663587104846650178, 3.286797332666310467 ) ) ;
#10196 = DIRECTION ( 'NONE',  ( 0.000000000000000000, 0.000000000000000000, 1.000000000000000000 ) ) ;
#10197 = CARTESIAN_POINT ( 'NONE',  ( 1.851400890972779045, -5.113135593220339281, 6.601359968904126241 ) ) ;
#10198 = ORIENTED_EDGE ( 'NONE', *, *, #14133, .F. ) ;
#10199 = DIRECTION ( 'NONE',  ( -0.000000000000000000, 1.000000000000000000, 0.000000000000000000 ) ) ;
#10200 = DIRECTION ( 'NONE',  ( 4.440892098500630106E-16, 0.000000000000000000, -1.000000000000000000 ) ) ;
#10201 = ORIENTED_EDGE ( 'NONE', *, *, #12205, .F. ) ;
#10202 = CARTESIAN_POINT ( 'NONE',  ( -1.889999999999999902, 7.299999999999999822, 0.6099999999999999867 ) ) ;
#10203 = FACE_OUTER_BOUND ( 'NONE', #4522, .T. ) ;
#10204 = CARTESIAN_POINT ( 'NONE',  ( 0.2993653819235879698, -2.914521003261450360, 6.731079075450741911 ) ) ;
#10205 = CARTESIAN_POINT ( 'NONE',  ( 2.601107615185130673, -0.3845338983050847759, 5.226397344856369642 ) ) ;
#10206 = ADVANCED_FACE ( 'NONE', ( #11325 ), #5680, .T. ) ;
#10207 = ORIENTED_EDGE ( 'NONE', *, *, #4729, .T. ) ;
#10208 = DIRECTION ( 'NONE',  ( -1.000000000000000000, 0.000000000000000000, 0.000000000000000000 ) ) ;
#10209 = DIRECTION ( 'NONE',  ( -1.142385477618690234E-14, 1.110223024625159992E-16, -1.000000000000000000 ) ) ;
#10210 = CARTESIAN_POINT ( 'NONE',  ( 1.202278654260740876, -0.4201271186440683758, 6.364093491318035589 ) ) ;
#10211 = EDGE_LOOP ( 'NONE', ( #12963, #695, #6150, #267 ) ) ;
#10212 = ORIENTED_EDGE ( 'NONE', *, *, #15608, .F. ) ;
#10213 = CARTESIAN_POINT ( 'NONE',  ( 0.1749999999999999889, 8.200000000000001066, -3.200000000000000178 ) ) ;
#10215 = CIRCLE ( 'NONE', #757, 1.000000000000000000 ) ;
#10214 = SURFACE_STYLE_USAGE ( .BOTH. , #7372 ) ;
#10216 = CARTESIAN_POINT ( 'NONE',  ( 0.1565249325564389560, -0.1468220338983060036, 7.048192310558507145 ) ) ;
#10217 = CARTESIAN_POINT ( 'NONE',  ( 0.009452110982654818305, -0.3001920447045379747, 2.350000000000000089 ) ) ;
#10218 = CARTESIAN_POINT ( 'NONE',  ( -1.011820239713360658, -3.636457940198391636, 2.246566997958110434 ) ) ;
#10219 = VERTEX_POINT ( 'NONE', #14197 ) ;
#10220 = CARTESIAN_POINT ( 'NONE',  ( -0.6673090596498669758, -3.360839357098900138, 2.443133963569589895 ) ) ;
#10221 = VECTOR ( 'NONE', #16658, 1000.000000000000000 ) ;
#10222 = LINE ( 'NONE', #3290, #12056 ) ;
#10223 = CARTESIAN_POINT ( 'NONE',  ( 0.9976707306414894783, -2.522460978720530989, 6.494311833503137343 ) ) ;
#10224 = VECTOR ( 'NONE', #11, 1000.000000000000000 ) ;
#10225 = DIRECTION ( 'NONE',  ( 0.000000000000000000, 0.000000000000000000, -1.000000000000000000 ) ) ;
#10226 = VECTOR ( 'NONE', #13370, 1000.000000000000000 ) ;
#10227 = ORIENTED_EDGE ( 'NONE', *, *, #6137, .T. ) ;
#10228 = CARTESIAN_POINT ( 'NONE',  ( -1.250000000000000000, 3.500000000000000000, 5.100000000000000533 ) ) ;
#10229 = CARTESIAN_POINT ( 'NONE',  ( 0.2908063684825958894, -1.055298816558370101, 7.337905485238597869 ) ) ;
#10230 = CARTESIAN_POINT ( 'NONE',  ( 0.1749999999999999889, 2.700000000000000178, 1.600000000000000089 ) ) ;
#10231 = CARTESIAN_POINT ( 'NONE',  ( 2.500000000000000000, 2.000000000000000000, 1.600000000000000089 ) ) ;
#10232 = DIRECTION ( 'NONE',  ( 0.7071067811865470176, 0.000000000000000000, -0.7071067811865480168 ) ) ;
#10233 = CARTESIAN_POINT ( 'NONE',  ( -1.128670402850159737, -5.170974576271189171, 7.101865548313641696 ) ) ;
#10234 = ORIENTED_EDGE ( 'NONE', *, *, #13946, .T. ) ;
#10235 = ORIENTED_EDGE ( 'NONE', *, *, #14124, .F. ) ;
#10236 = CARTESIAN_POINT ( 'NONE',  ( 2.500000000000000000, 2.000000000000000000, -1.522591576628789972E-15 ) ) ;
#10237 = FACE_OUTER_BOUND ( 'NONE', #13129, .T. ) ;
#10238 = VERTEX_POINT ( 'NONE', #15687 ) ;
#10239 = VECTOR ( 'NONE', #1974, 1000.000000000000000 ) ;
#10240 = AXIS2_PLACEMENT_3D ( 'NONE', #17472, #17553, #10531 ) ;
#10241 = LINE ( 'NONE', #12856, #3510 ) ;
#10242 = CARTESIAN_POINT ( 'NONE',  ( -2.197904923864619331, -3.193980462720909408, 6.187389538303117220 ) ) ;
#10243 = EDGE_CURVE ( 'NONE', #2335, #5031, #14285, .T. ) ;
#10244 = FACE_OUTER_BOUND ( 'NONE', #12892, .T. ) ;
#10245 = LINE ( 'NONE', #171, #6714 ) ;
#10246 = EDGE_CURVE ( 'NONE', #2515, #15551, #13589, .T. ) ;
#10247 = CIRCLE ( 'NONE', #6158, 0.5999999999999998668 ) ;
#10248 = CARTESIAN_POINT ( 'NONE',  ( -1.526791597786389953, -2.825208726468269926, 6.490992212270280781 ) ) ;
#10249 = AXIS2_PLACEMENT_3D ( 'NONE', #13391, #526, #12004 ) ;
#10250 = DIRECTION ( 'NONE',  ( 0.000000000000000000, 0.000000000000000000, 1.000000000000000000 ) ) ;
#10251 = CARTESIAN_POINT ( 'NONE',  ( -1.930452136971070987, -1.587088570829020551, 6.521117305355617511 ) ) ;
#10252 = PLANE ( 'NONE',  #17023 ) ;
#10253 = CARTESIAN_POINT ( 'NONE',  ( 1.224086244040949900, -4.358394877135324030, 6.348185277745746369 ) ) ;
#10254 = VECTOR ( 'NONE', #9792, 1000.000000000000000 ) ;
#10255 = LINE ( 'NONE', #17111, #4378 ) ;
#10256 = VECTOR ( 'NONE', #4328, 1000.000000000000227 ) ;
#10257 = DIRECTION ( 'NONE',  ( 1.000000000000000000, -1.224646799147339895E-16, 0.000000000000000000 ) ) ;
#10258 = ORIENTED_EDGE ( 'NONE', *, *, #13431, .F. ) ;
#10259 = CARTESIAN_POINT ( 'NONE',  ( -1.399999999999999911, -9.500000000000000000, 3.299999999999999822 ) ) ;
#10260 = VERTEX_POINT ( 'NONE', #14545 ) ;
#10261 = DIRECTION ( 'NONE',  ( -1.000000000000000000, -1.306144734853119962E-16, 0.000000000000000000 ) ) ;
#10262 = VECTOR ( 'NONE', #15761, 1000.000000000000000 ) ;
#10263 = PLANE ( 'NONE',  #3203 ) ;
#10264 = VECTOR ( 'NONE', #13810, 1000.000000000000000 ) ;
#10265 = VECTOR ( 'NONE', #206, 1000.000000000000000 ) ;
#10266 = ADVANCED_FACE ( 'NONE', ( #388 ), #13246, .T. ) ;
#10267 = ORIENTED_EDGE ( 'NONE', *, *, #16171, .F. ) ;
#10268 = CARTESIAN_POINT ( 'NONE',  ( -0.06367493584607197832, -5.298516949152545230, 2.649999999999998579 ) ) ;
#10269 = CARTESIAN_POINT ( 'NONE',  ( -0.3752419433106839453, -1.424070552810999812, 7.023346545710370314 ) ) ;
#10270 = CARTESIAN_POINT ( 'NONE',  ( -2.065789008932981119, -2.871785303044851023, 6.366022047745341084 ) ) ;
#10271 = EDGE_CURVE ( 'NONE', #6491, #9952, #11866, .T. ) ;
#10272 = AXIS2_PLACEMENT_3D ( 'NONE', #3735, #17707, #886 ) ;
#10273 =( NAMED_UNIT ( * ) PLANE_ANGLE_UNIT ( ) SI_UNIT ( $, .RADIAN. ) );
#10274 = VECTOR ( 'NONE', #8316, 1000.000000000000000 ) ;
#10275 = ADVANCED_FACE ( 'NONE', ( #14719 ), #9062, .T. ) ;
#10276 = CARTESIAN_POINT ( 'NONE',  ( -1.699999999999999956, 9.299999999999998934, 7.700000000000000178 ) ) ;
#10277 = EDGE_CURVE ( 'NONE', #5830, #10219, #16115, .T. ) ;
#10278 = CARTESIAN_POINT ( 'NONE',  ( 1.704669856830330010, -0.8030495317899829510, 3.080704711052640210 ) ) ;
#10279 = CARTESIAN_POINT ( 'NONE',  ( -1.250000000000000000, 7.799999999999999822, 5.100000000000000533 ) ) ;
#10280 = CARTESIAN_POINT ( 'NONE',  ( -2.325590009395030133, -4.870737219477670799, 5.061077271074069905 ) ) ;
#10281 = EDGE_CURVE ( 'NONE', #1367, #5117, #17298, .T. ) ;
#10282 = CARTESIAN_POINT ( 'NONE',  ( 1.043047520545210105, -4.082776294035843634, 6.468319459971126228 ) ) ;
#10283 = AXIS2_PLACEMENT_3D ( 'NONE', #9818, #5289, #5382 ) ;
#10284 = LINE ( 'NONE', #9928, #14706 ) ;
#10285 = CARTESIAN_POINT ( 'NONE',  ( -1.800000000000000044, 0.5999999999999999778, 1.600000000000000089 ) ) ;
#10286 = ORIENTED_EDGE ( 'NONE', *, *, #8461, .F. ) ;
#10287 = CIRCLE ( 'NONE', #5858, 0.6999999999999992895 ) ;
#10288 = EDGE_CURVE ( 'NONE', #8504, #15242, #9164, .T. ) ;
#10289 = CARTESIAN_POINT ( 'NONE',  ( -0.4339619423229766348, -0.1601694915254239793, 6.706578715862737461 ) ) ;
#10290 = CARTESIAN_POINT ( 'NONE',  ( 0.9719602541832789155, -2.844656138396589817, 6.843370931913530519 ) ) ;
#10291 = AXIS2_PLACEMENT_3D ( 'NONE', #13423, #11574, #16111 ) ;
#10292 = VERTEX_POINT ( 'NONE', #14463 ) ;
#10293 = ORIENTED_EDGE ( 'NONE', *, *, #15938, .T. ) ;
#10294 = DIRECTION ( 'NONE',  ( 1.000000000000000000, 0.000000000000000000, 0.000000000000000000 ) ) ;
#10295 = ORIENTED_EDGE ( 'NONE', *, *, #11970, .F. ) ;
#10296 = CARTESIAN_POINT ( 'NONE',  ( -1.115198193348239997, -4.338947465207011689, 6.772457159276568994 ) ) ;
#10297 = CIRCLE ( 'NONE', #5879, 0.4999999999999995559 ) ;
#10298 = DIRECTION ( 'NONE',  ( 1.000000000000000000, 0.000000000000000000, 0.000000000000000000 ) ) ;
#10299 = CARTESIAN_POINT ( 'NONE',  ( -0.2469343877495291661, -5.595550847457635868, 2.057675570509529539 ) ) ;
#10300 = AXIS2_PLACEMENT_3D ( 'NONE', #2216, #551, #828 ) ;
#10301 = ADVANCED_FACE ( 'NONE', ( #13154 ), #3335, .F. ) ;
#10302 = ORIENTED_EDGE ( 'NONE', *, *, #3351, .F. ) ;
#10303 = CARTESIAN_POINT ( 'NONE',  ( 1.889999999999999902, 8.500000000000000000, 0.6099999999999999867 ) ) ;
#10304 = CARTESIAN_POINT ( 'NONE',  ( -0.7093417302541390468, -0.4646186440677970153, 6.943956659919700236 ) ) ;
#10305 = EDGE_LOOP ( 'NONE', ( #1584, #15655 ) ) ;
#10306 = VECTOR ( 'NONE', #7806, 1000.000000000000114 ) ;
#10307 = CARTESIAN_POINT ( 'NONE',  ( 1.899999999999999911, 9.199999999999999289, 1.600000000000000089 ) ) ;
#10308 = DIRECTION ( 'NONE',  ( 0.000000000000000000, 0.000000000000000000, -1.000000000000000000 ) ) ;
#10309 = CARTESIAN_POINT ( 'NONE',  ( -1.668733558229350766, -4.754295778036219389, 5.895922302771936074 ) ) ;
#10310 = CARTESIAN_POINT ( 'NONE',  ( 0.1765068388402390998, -0.4468220338983063811, 7.347961541693647902 ) ) ;
#10311 = ORIENTED_EDGE ( 'NONE', *, *, #11047, .T. ) ;
#10312 = DIRECTION ( 'NONE',  ( 0.000000000000000000, 0.000000000000000000, 1.000000000000000000 ) ) ;
#10313 = CARTESIAN_POINT ( 'NONE',  ( 1.000000000000000000, -7.000000000000000000, 3.700000000000000178 ) ) ;
#10314 = VECTOR ( 'NONE', #2896, 1000.000000000000000 ) ;
#10315 = ADVANCED_FACE ( 'NONE', ( #3413 ), #10371, .T. ) ;
#10316 = ORIENTED_EDGE ( 'NONE', *, *, #5074, .T. ) ;
#10317 = CARTESIAN_POINT ( 'NONE',  ( -0.009452110982655708218, -0.5998079552954630467, 2.350000000000000089 ) ) ;
#10318 = CARTESIAN_POINT ( 'NONE',  ( -0.1910247150515231307, -5.595550847457635868, 2.655937705488500722 ) ) ;
#10319 = EDGE_CURVE ( 'NONE', #7625, #4727, #3254, .T. ) ;
#10320 = CARTESIAN_POINT ( 'NONE',  ( -0.7093417302541388247, -0.1646186440677969709, 6.943956659919700236 ) ) ;
#10321 = CARTESIAN_POINT ( 'NONE',  ( 2.248786803694151182, -4.265241723982168942, 6.109280527266637506 ) ) ;
#10322 = EDGE_CURVE ( 'NONE', #12793, #17050, #4897, .T. ) ;
#10323 = EDGE_LOOP ( 'NONE', ( #9845, #13499, #5775, #16971 ) ) ;
#10324 = AXIS2_PLACEMENT_3D ( 'NONE', #304, #1687, #8550 ) ;
#10325 = CARTESIAN_POINT ( 'NONE',  ( -2.211317922628890376, -3.127956474216019966, 3.894507149290469705 ) ) ;
#10326 = LINE ( 'NONE', #13185, #771 ) ;
#10327 = CARTESIAN_POINT ( 'NONE',  ( -4.404543739248539922E-17, 5.113553479078069230, 6.680683419527140288 ) ) ;
#10328 = CARTESIAN_POINT ( 'NONE',  ( 2.051695471449629160, -2.266289807549351387, 4.773807418740724451 ) ) ;
#10329 = CARTESIAN_POINT ( 'NONE',  ( -0.3042893218813459977, 3.050000000000000266, 2.029289321881350361 ) ) ;
#10330 = ORIENTED_EDGE ( 'NONE', *, *, #16488, .T. ) ;
#10331 = DIRECTION ( 'NONE',  ( 9.349246523159200620E-16, 0.000000000000000000, -1.000000000000000000 ) ) ;
#10332 = CARTESIAN_POINT ( 'NONE',  ( 2.622715975066190364, -0.7292627805223297344, 5.105554690682975405 ) ) ;
#10333 = ORIENTED_EDGE ( 'NONE', *, *, #3351, .T. ) ;
#10334 = CIRCLE ( 'NONE', #5621, 0.2750000000000000222 ) ;
#10335 = CARTESIAN_POINT ( 'NONE',  ( 0.4005155088302400634, -4.474836318576759453, 7.019123328904770531 ) ) ;
#10336 = DIRECTION ( 'NONE',  ( -1.000000000000000000, 0.000000000000000000, 0.000000000000000000 ) ) ;
#10337 = DIRECTION ( 'NONE',  ( 0.000000000000000000, 0.000000000000000000, -1.000000000000000000 ) ) ;
#10338 = EDGE_LOOP ( 'NONE', ( #15698, #6860, #15301, #5896 ) ) ;
#10339 = ORIENTED_EDGE ( 'NONE', *, *, #17844, .F. ) ;
#10340 = DIRECTION ( 'NONE',  ( 1.632680918566409751E-16, -1.000000000000000000, 0.000000000000000000 ) ) ;
#10341 = DIRECTION ( 'NONE',  ( 1.000000000000000000, -2.220446049250309876E-16, -6.049014748177260544E-16 ) ) ;
#10342 = EDGE_LOOP ( 'NONE', ( #13722, #3323, #12262 ) ) ;
#10343 = DIRECTION ( 'NONE',  ( -6.161988852941170860E-64, -1.000000000000000000, 3.773129962568039733E-80 ) ) ;
#10344 = CARTESIAN_POINT ( 'NONE',  ( 0.9880847989278174204, -2.262448931189378509, 2.236912075639679198 ) ) ;
#10345 = CARTESIAN_POINT ( 'NONE',  ( 1.545075033357670158, -0.4774152569121719591, 2.920238509828300355 ) ) ;
#10346 = PLANE ( 'NONE',  #17340 ) ;
#10347 = AXIS2_PLACEMENT_3D ( 'NONE', #17806, #3653, #8033 ) ;
#10348 = CARTESIAN_POINT ( 'NONE',  ( -1.832842064134660109, -2.871785303044850135, 6.176291182464519913 ) ) ;
#10349 = CARTESIAN_POINT ( 'NONE',  ( 1.661700935788380074, -5.337500000000000355, 3.038299064211610112 ) ) ;
#10350 = CARTESIAN_POINT ( 'NONE',  ( -0.9038768003981948462, -1.470647129387581575, 7.195219513931347954 ) ) ;
#10351 = LINE ( 'NONE', #1845, #7282 ) ;
#10352 = CARTESIAN_POINT ( 'NONE',  ( -1.668733558229350766, -4.754295778036219389, 5.895922302771936074 ) ) ;
#10353 = DIRECTION ( 'NONE',  ( -4.440892098500630106E-16, -1.000000000000000000, -1.332267629550190018E-15 ) ) ;
#10354 = ORIENTED_EDGE ( 'NONE', *, *, #7501, .F. ) ;
#10355 = DIRECTION ( 'NONE',  ( -0.000000000000000000, 1.000000000000000000, 0.000000000000000000 ) ) ;
#10356 = ORIENTED_EDGE ( 'NONE', *, *, #8793, .T. ) ;
#10357 = EDGE_CURVE ( 'NONE', #2437, #11376, #17402, .T. ) ;
#10358 = DIRECTION ( 'NONE',  ( 1.306144734853129823E-16, -1.000000000000000000, 0.000000000000000000 ) ) ;
#10359 = AXIS2_PLACEMENT_3D ( 'NONE', #12676, #18106, #16835 ) ;
#10360 = DIRECTION ( 'NONE',  ( -4.318427418585891014E-15, 2.220446049250309876E-16, -1.000000000000000000 ) ) ;
#10361 = ORIENTED_EDGE ( 'NONE', *, *, #4770, .T. ) ;
#10362 = CARTESIAN_POINT ( 'NONE',  ( 2.352760675243219968, -2.565196678937129882, 4.757121734156020132 ) ) ;
#10363 = CARTESIAN_POINT ( 'NONE',  ( 2.350067830300900162, -5.377542372881360500, 4.825253242917690422 ) ) ;
#10364 = CARTESIAN_POINT ( 'NONE',  ( -3.763524982345449879E-15, -5.450000000000000178, 2.350000000000000089 ) ) ;
#10365 = CARTESIAN_POINT ( 'NONE',  ( -2.182690844914350059, -1.680241723982170088, 5.580117243900479806 ) ) ;
#10366 = VECTOR ( 'NONE', #16678, 1000.000000000000000 ) ;
#10367 = CARTESIAN_POINT ( 'NONE',  ( 2.313035575219750228, -4.172088570829020071, 5.134294963419709923 ) ) ;
#10368 = CARTESIAN_POINT ( 'NONE',  ( 2.033547680391670998, -0.9583047870452394701, 4.417890669792418734 ) ) ;
#10369 = EDGE_CURVE ( 'NONE', #14203, #10460, #10549, .T. ) ;
#10370 = DIRECTION ( 'NONE',  ( -2.114710523095539848E-16, -1.000000000000000000, 0.000000000000000000 ) ) ;
#10371 = PLANE ( 'NONE',  #7387 ) ;
#10372 = ORIENTED_EDGE ( 'NONE', *, *, #11854, .T. ) ;
#10373 = ADVANCED_FACE ( 'NONE', ( #17485 ), #10454, .T. ) ;
#10374 = CARTESIAN_POINT ( 'NONE',  ( 1.846259792136599076, -0.3533898305084745561, 3.802221692020924415 ) ) ;
#10375 = CARTESIAN_POINT ( 'NONE',  ( 1.026235786675480099, -4.404971453711899798, 6.817920158464540137 ) ) ;
#10376 = ORIENTED_EDGE ( 'NONE', *, *, #13112, .F. ) ;
#10377 = EDGE_CURVE ( 'NONE', #2805, #13228, #4534, .T. ) ;
#10378 = EDGE_LOOP ( 'NONE', ( #799, #6996, #18157, #16351 ) ) ;
#10379 = EDGE_CURVE ( 'NONE', #15324, #1696, #14824, .T. ) ;
#10380 = CARTESIAN_POINT ( 'NONE',  ( 1.399999999999999911, 5.799999999999999822, 7.700000000000000178 ) ) ;
#10381 = VERTEX_POINT ( 'NONE', #13429 ) ;
#10382 = CARTESIAN_POINT ( 'NONE',  ( -2.276802572547989456, -3.104668185927729862, 4.104251954998811236 ) ) ;
#10383 = ITEM_DEFINED_TRANSFORMATION ( 'NONE', 'NONE', #3505,  #17681 ) ;
#10384 = CARTESIAN_POINT ( 'NONE',  ( -0.9664230948142090716, -5.582203389830510787, 2.228384861502259895 ) ) ;
#10385 = LINE ( 'NONE', #17226, #5847 ) ;
#10386 = CARTESIAN_POINT ( 'NONE',  ( -2.500000000000000000, 7.299999999999999822, 1.600000000000000089 ) ) ;
#10387 = ORIENTED_EDGE ( 'NONE', *, *, #11938, .T. ) ;
#10388 = LINE ( 'NONE', #7710, #17911 ) ;
#10389 = FACE_OUTER_BOUND ( 'NONE', #1866, .T. ) ;
#10390 = CARTESIAN_POINT ( 'NONE',  ( 1.909909196654749897, -4.032358841099289215, 3.946907241329673521 ) ) ;
#10391 = CARTESIAN_POINT ( 'NONE',  ( 1.399999999999999911, -6.000000000000000000, 3.299999999999999822 ) ) ;
#10392 = CARTESIAN_POINT ( 'NONE',  ( 2.458531667407859889, -0.09343220338983100615, 5.699238225248945966 ) ) ;
#10393 = ORIENTED_EDGE ( 'NONE', *, *, #7000, .T. ) ;
#10394 = CARTESIAN_POINT ( 'NONE',  ( 0.6493550500446280127, -0.3133474576271190193, 2.437955526623099889 ) ) ;
#10395 = EDGE_CURVE ( 'NONE', #10948, #9933, #742, .T. ) ;
#10396 = VERTEX_POINT ( 'NONE', #1031 ) ;
#10397 = LINE ( 'NONE', #17071, #15411 ) ;
#10398 = CARTESIAN_POINT ( 'NONE',  ( 0.5921572875253799939, 3.050000000000000266, 1.600000000000000089 ) ) ;
#10399 = DIRECTION ( 'NONE',  ( 1.168655815394900078E-16, -1.000000000000000000, -5.843279076974510248E-17 ) ) ;
#10400 = CARTESIAN_POINT ( 'NONE',  ( 2.500000000000000000, 0.4000000000000000222, 7.649999999999999467 ) ) ;
#10401 = PRESENTATION_LAYER_ASSIGNMENT (  '', '', ( #6009 ) ) ;
#10402 = CARTESIAN_POINT ( 'NONE',  ( -2.049607015837349167, -3.170692174432623744, 6.385889905549041679 ) ) ;
#10403 = ORIENTED_EDGE ( 'NONE', *, *, #11147, .F. ) ;
#10404 = CARTESIAN_POINT ( 'NONE',  ( -0.01716182025094739952, -3.430704221963770006, 2.346608583467349796 ) ) ;
#10405 = CARTESIAN_POINT ( 'NONE',  ( -0.6500000000000000222, 6.450000000000000178, 2.699264068711930253 ) ) ;
#10406 = CARTESIAN_POINT ( 'NONE',  ( 0.5999999999999999778, -7.347880794884110368E-17, 7.700000000000000178 ) ) ;
#10407 = CARTESIAN_POINT ( 'NONE',  ( -1.785776242921159884, -4.478677194936736328, 5.712869711683835838 ) ) ;
#10408 = DIRECTION ( 'NONE',  ( -1.000000000000000000, 0.000000000000000000, 0.000000000000000000 ) ) ;
#10409 = CARTESIAN_POINT ( 'NONE',  ( -2.043688444617268729, -1.497776294035840561, 4.504451070148879133 ) ) ;
#10410 = ORIENTED_EDGE ( 'NONE', *, *, #17839, .T. ) ;
#10411 = DIRECTION ( 'NONE',  ( 0.000000000000000000, 0.000000000000000000, 1.000000000000000000 ) ) ;
#10412 = EDGE_CURVE ( 'NONE', #13022, #13413, #6186, .T. ) ;
#10413 = LINE ( 'NONE', #13117, #5285 ) ;
#10414 = CARTESIAN_POINT ( 'NONE',  ( -2.369027826908540302, -1.590929447188999646, 3.503830760997904470 ) ) ;
#10415 = VECTOR ( 'NONE', #5337, 1000.000000000000000 ) ;
#10416 = ORIENTED_EDGE ( 'NONE', *, *, #10722, .T. ) ;
#10417 = CARTESIAN_POINT ( 'NONE',  ( 1.571912189623089873, -4.335106588847041031, 6.451524409078630562 ) ) ;
#10418 = CARTESIAN_POINT ( 'NONE',  ( 1.800000000000000044, 0.5999999999999999778, 6.599999999999999645 ) ) ;
#10419 = CARTESIAN_POINT ( 'NONE',  ( 0.1749999999999999889, 6.799999999999999822, 1.600000000000000089 ) ) ;
#10420 = CARTESIAN_POINT ( 'NONE',  ( -2.180207327701300102, -5.206567796610169552, 5.586116916730199833 ) ) ;
#10421 = ORIENTED_EDGE ( 'NONE', *, *, #8796, .T. ) ;
#10422 = ORIENTED_EDGE ( 'NONE', *, *, #5696, .T. ) ;
#10423 = DIRECTION ( 'NONE',  ( 0.7071067811865489050, 0.000000000000000000, 0.7071067811865460184 ) ) ;
#10424 =( NAMED_UNIT ( * ) SI_UNIT ( $, .STERADIAN. ) SOLID_ANGLE_UNIT ( ) );
#10425 = FACE_OUTER_BOUND ( 'NONE', #15839, .T. ) ;
#10426 = VERTEX_POINT ( 'NONE', #6377 ) ;
#10427 = CARTESIAN_POINT ( 'NONE',  ( -2.260671505268489145, -1.913124606865061139, 3.309864021662289435 ) ) ;
#10428 = CARTESIAN_POINT ( 'NONE',  ( 1.118481890237429610, -0.4076464065212261345, 2.289482119763390333 ) ) ;
#10429 = CIRCLE ( 'NONE', #7483, 0.04999999999999991257 ) ;
#10430 = DIRECTION ( 'NONE',  ( 1.000000000000000000, 4.014365738757630620E-15, 5.017957173447030386E-16 ) ) ;
#10431 = CARTESIAN_POINT ( 'NONE',  ( 0.1569242594330760021, -4.199217735477280833, 7.048216443236290374 ) ) ;
#10432 = CARTESIAN_POINT ( 'NONE',  ( 1.340185291429730974, -5.033893599512585304, 3.140995886557053307 ) ) ;
#10433 = CARTESIAN_POINT ( 'NONE',  ( 2.626509418457480649, -1.028169651910100679, 5.080213055741780614 ) ) ;
#10434 = AXIS2_PLACEMENT_3D ( 'NONE', #6270, #13407, #13502 ) ;
#10435 = DIRECTION ( 'NONE',  ( 1.000000000000000000, 0.000000000000000000, 0.000000000000000000 ) ) ;
#10436 = CARTESIAN_POINT ( 'NONE',  ( 2.306642602145299925, -0.3845338983050849979, 5.166805192608480368 ) ) ;
#10437 = CARTESIAN_POINT ( 'NONE',  ( 1.000000000000000000, 6.799999999999999822, 8.300000000000000711 ) ) ;
#10438 = CARTESIAN_POINT ( 'NONE',  ( -1.707817112497179934, -5.488771186440679628, 6.319218296629480314 ) ) ;
#10439 = ORIENTED_EDGE ( 'NONE', *, *, #5373, .T. ) ;
#10440 = VECTOR ( 'NONE', #18140, 1000.000000000000000 ) ;
#10441 = DIRECTION ( 'NONE',  ( -1.734723475976809806E-16, 1.000000000000000000, 0.000000000000000000 ) ) ;
#10442 = EDGE_LOOP ( 'NONE', ( #4211, #5905, #6237, #11300, #6217, #10393, #11166, #17851 ) ) ;
#10443 = CARTESIAN_POINT ( 'NONE',  ( 4.225031457058369810E-16, 2.299999999999999822, 7.599999999999999645 ) ) ;
#10444 = PLANE ( 'NONE',  #15344 ) ;
#10445 = EDGE_LOOP ( 'NONE', ( #2941, #1147, #10159, #8077 ) ) ;
#10446 = CARTESIAN_POINT ( 'NONE',  ( -2.005512128484160161, -1.913124606865060029, 3.468469736471389897 ) ) ;
#10447 = FILL_AREA_STYLE_COLOUR ( '', #9676 ) ;
#10448 = LINE ( 'NONE', #558, #11749 ) ;
#10449 = CARTESIAN_POINT ( 'NONE',  ( 6.661338147750939243E-16, 3.500000000000000000, 5.100000000000000533 ) ) ;
#10450 = PLANE ( 'NONE',  #10291 ) ;
#10451 = CARTESIAN_POINT ( 'NONE',  ( 1.214457691475989920, -3.869340823081270031, 2.684103622926340194 ) ) ;
#10452 = CARTESIAN_POINT ( 'NONE',  ( 1.292934267244360447, -1.214475958216409746, 6.294748514096617065 ) ) ;
#10453 = CARTESIAN_POINT ( 'NONE',  ( -4.592425496802605650E-17, 2.550000000000000266, 7.700000000000000178 ) ) ;
#10454 = PLANE ( 'NONE',  #12409 ) ;
#10455 = VERTEX_POINT ( 'NONE', #12416 ) ;
#10456 = DIRECTION ( 'NONE',  ( 3.700743415417190309E-15, -6.579099405186109509E-16, 1.000000000000000000 ) ) ;
#10457 = CARTESIAN_POINT ( 'NONE',  ( 1.526871680339569659, -0.3400423728813561364, 3.327650196883443101 ) ) ;
#10458 = CARTESIAN_POINT ( 'NONE',  ( -1.781655196750479897, -3.520016498756949996, 3.162323035427820450 ) ) ;
#10459 = CIRCLE ( 'NONE', #6626, 0.5999999999999999778 ) ;
#10460 = VERTEX_POINT ( 'NONE', #6577 ) ;
#10461 = ORIENTED_EDGE ( 'NONE', *, *, #5410, .T. ) ;
#10462 = CARTESIAN_POINT ( 'NONE',  ( -0.5372984490435469551, 4.250000000000000000, 8.300000000000000711 ) ) ;
#10463 = ORIENTED_EDGE ( 'NONE', *, *, #3584, .F. ) ;
#10464 = DIRECTION ( 'NONE',  ( -1.000000000000000000, 0.000000000000000000, -2.400482215405740060E-16 ) ) ;
#10465 = ITEM_DEFINED_TRANSFORMATION ( 'NONE', 'NONE', #1751,  #17681 ) ;
#10466 = CARTESIAN_POINT ( 'NONE',  ( -2.268288188848061715, -5.251059322033895249, 3.322421079292323665 ) ) ;
#10467 = PLANE ( 'NONE',  #14119 ) ;
#10468 = LINE ( 'NONE', #15867, #4927 ) ;
#10469 = ORIENTED_EDGE ( 'NONE', *, *, #1258, .T. ) ;
#10470 = ADVANCED_FACE ( 'NONE', ( #9456 ), #10941, .T. ) ;
#10471 = CARTESIAN_POINT ( 'NONE',  ( 1.800000000000000044, 11.29999999999999893, 7.649999999999999467 ) ) ;
#10472 =( GEOMETRIC_REPRESENTATION_CONTEXT ( 3 ) GLOBAL_UNCERTAINTY_ASSIGNED_CONTEXT ( ( #12511 ) ) GLOBAL_UNIT_ASSIGNED_CONTEXT ( ( #2497, #9329, #13704 ) ) REPRESENTATION_CONTEXT ( 'NONE', 'WORKASPACE' ) );
#10473 = EDGE_CURVE ( 'NONE', #4745, #4957, #6484, .T. ) ;
#10474 = CARTESIAN_POINT ( 'NONE',  ( 1.835037444103841286, -4.241953435693877061, 5.620619042473564697 ) ) ;
#10475 = ADVANCED_FACE ( 'NONE', ( #5005 ), #9629, .F. ) ;
#10476 = CARTESIAN_POINT ( 'NONE',  ( 2.601107615185130673, -0.08453389830508521718, 5.226397344856369642 ) ) ;
#10477 = ORIENTED_EDGE ( 'NONE', *, *, #15498, .F. ) ;
#10478 = CARTESIAN_POINT ( 'NONE',  ( 1.428515267734870031, -0.3311440677966109858, 2.829745655876919841 ) ) ;
#10479 = VERTEX_POINT ( 'NONE', #10658 ) ;
#10480 = CARTESIAN_POINT ( 'NONE',  ( -1.932035991685910004, -0.5610169491525425212, 2.884370051397200818 ) ) ;
#10481 = ORIENTED_EDGE ( 'NONE', *, *, #9182, .F. ) ;
#10482 = DIRECTION ( 'NONE',  ( 0.000000000000000000, 6.123233995736769734E-17, -1.000000000000000000 ) ) ;
#10483 = DIRECTION ( 'NONE',  ( 1.000000000000000000, -1.059337802663170094E-14, 1.821459649775649668E-16 ) ) ;
#10484 = CARTESIAN_POINT ( 'NONE',  ( -0.1698804968610999888, -0.2965485159365569556, 2.349238660949160007 ) ) ;
#10485 = CARTESIAN_POINT ( 'NONE',  ( -2.197904923864619331, -3.193980462720909408, 6.187389538303117220 ) ) ;
#10486 = ORIENTED_EDGE ( 'NONE', *, *, #9369, .F. ) ;
#10487 = EDGE_CURVE ( 'NONE', #5830, #6456, #7981, .T. ) ;
#10488 = CARTESIAN_POINT ( 'NONE',  ( -2.126557263589650137, -3.151244762504310071, 3.691783806836059778 ) ) ;
#10489 = EDGE_CURVE ( 'NONE', #17764, #14464, #16672, .T. ) ;
#10490 = LINE ( 'NONE', #8610, #5185 ) ;
#10491 = ADVANCED_FACE ( 'NONE', ( #2510 ), #7713, .T. ) ;
#10492 = CARTESIAN_POINT ( 'NONE',  ( 1.978802102381368888, -3.756740257999804378, 4.152967933079626306 ) ) ;
#10493 = CARTESIAN_POINT ( 'NONE',  ( -1.899999999999999911, 8.500000000000000000, 0.6099999999999999867 ) ) ;
#10494 = LINE ( 'NONE', #17251, #15063 ) ;
#10495 = CARTESIAN_POINT ( 'NONE',  ( -0.5302109551885640926, -1.800524041783588824, 2.716624547488271979 ) ) ;
#10496 = ORIENTED_EDGE ( 'NONE', *, *, #5521, .T. ) ;
#10497 = FACE_OUTER_BOUND ( 'NONE', #10792, .T. ) ;
#10498 = DIRECTION ( 'NONE',  ( 2.960594732333750117E-16, -1.000000000000000000, 0.000000000000000000 ) ) ;
#10499 = CARTESIAN_POINT ( 'NONE',  ( 0.5355577887186364627, -1.032010528270079330, 7.299286738308158107 ) ) ;
#10500 = ORIENTED_EDGE ( 'NONE', *, *, #16602, .F. ) ;
#10501 = DIRECTION ( 'NONE',  ( -9.349246523159200620E-16, 0.000000000000000000, -1.000000000000000000 ) ) ;
#10502 = CARTESIAN_POINT ( 'NONE',  ( -1.899999999999999911, 9.199999999999999289, 0.6099999999999999867 ) ) ;
#10503 = CARTESIAN_POINT ( 'NONE',  ( -0.6628679656440369383, 6.450000000000000178, 1.670710678118660031 ) ) ;
#10504 = CARTESIAN_POINT ( 'NONE',  ( -0.2189795514005259958, -5.295550847457629828, 2.356806637999020015 ) ) ;
#10505 = VERTEX_POINT ( 'NONE', #9820 ) ;
#10506 = ORIENTED_EDGE ( 'NONE', *, *, #17058, .T. ) ;
#10507 = CARTESIAN_POINT ( 'NONE',  ( -1.875000000000000000, 2.296212748401290437E-16, 7.700000000000000178 ) ) ;
#10508 = CARTESIAN_POINT ( 'NONE',  ( 0.1749999999999999889, 7.700000000000000178, 1.600000000000000089 ) ) ;
#10509 = DIRECTION ( 'NONE',  ( 1.000000000000000000, 0.000000000000000000, 0.000000000000000000 ) ) ;
#10510 = ORIENTED_EDGE ( 'NONE', *, *, #8134, .F. ) ;
#10511 = DIRECTION ( 'NONE',  ( 1.110223024625159992E-16, -1.000000000000000000, 0.000000000000000000 ) ) ;
#10512 = CARTESIAN_POINT ( 'NONE',  ( 2.445954350973281510, -2.658349832090279197, 5.729767452368150771 ) ) ;
#10513 = ADVANCED_FACE ( 'NONE', ( #8430 ), #16, .F. ) ;
#10514 = DIRECTION ( 'NONE',  ( 0.000000000000000000, 0.000000000000000000, 1.000000000000000000 ) ) ;
#10515 = DIRECTION ( 'NONE',  ( 6.083413833562510128E-16, -9.455524548882000146E-32, 1.000000000000000000 ) ) ;
#10516 = AXIS2_PLACEMENT_3D ( 'NONE', #8975, #1676, #382 ) ;
#10517 = CARTESIAN_POINT ( 'NONE',  ( 1.981271652668330052, -3.966334852594400662, 5.970160748022399488 ) ) ;
#10518 = CARTESIAN_POINT ( 'NONE',  ( 0.9788656693287738353, -5.320452325212859712, 2.556357798777459944 ) ) ;
#10520 = ORIENTED_EDGE ( 'NONE', *, *, #14277, .F. ) ;
#10519 = CARTESIAN_POINT ( 'NONE',  ( 1.923406176634910203, -0.8030495317899833951, 2.875176962145290727 ) ) ;
#10521 = LINE ( 'NONE', #13405, #4084 ) ;
#10522 = FACE_OUTER_BOUND ( 'NONE', #16086, .T. ) ;
#10523 = CARTESIAN_POINT ( 'NONE',  ( 2.180207327701309872, -0.3934322033898309812, 5.586116916730190063 ) ) ;
#10524 = CARTESIAN_POINT ( 'NONE',  ( 0.6628679656440349399, 3.050000000000000266, 1.670710678118660031 ) ) ;
#10525 = ORIENTED_EDGE ( 'NONE', *, *, #11105, .T. ) ;
#10526 = CLOSED_SHELL ( 'NONE', ( #9745, #11186, #12492, #7686, #1213, #4360, #12535, #14753, #3386, #16575, #2512, #10883, #9945, #3984, #11730, #15817, #7953, #561, #11947, #15146, #16516, #9536, #16848, #13331, #6523, #3153, #3262, #3459, #11920, #472 ) ) ;
#10527 = AXIS2_PLACEMENT_3D ( 'NONE', #5872, #17059, #4549 ) ;
#10528 = EDGE_CURVE ( 'NONE', #12817, #13575, #2877, .T. ) ;
#10529 = CARTESIAN_POINT ( 'NONE',  ( 0.1749999999999999889, 9.299999999999998934, 1.600000000000000089 ) ) ;
#10530 = ORIENTED_EDGE ( 'NONE', *, *, #16850, .T. ) ;
#10531 = DIRECTION ( 'NONE',  ( 0.000000000000000000, 1.000000000000000000, -2.168404344971008868E-15 ) ) ;
#10532 = CARTESIAN_POINT ( 'NONE',  ( 1.899999999999999911, 10.00000000000000000, -5.075305255429290705E-16 ) ) ;
#10533 = EDGE_LOOP ( 'NONE', ( #16073, #14854, #3115, #14588 ) ) ;
#10534 = CIRCLE ( 'NONE', #4041, 1.000000000000000000 ) ;
#10535 = CARTESIAN_POINT ( 'NONE',  ( -0.6343239990445920240, -2.099430913171359769, 2.433641963034089972 ) ) ;
#10536 = EDGE_CURVE ( 'NONE', #16922, #1039, #12696, .T. ) ;
#10537 = CARTESIAN_POINT ( 'NONE',  ( -0.3743405594629430344, -5.457627118644070130, 7.023440622744399953 ) ) ;
#10538 = CARTESIAN_POINT ( 'NONE',  ( 1.750000000000000000, 11.40000000000000036, 7.550000000000000711 ) ) ;
#10539 = VECTOR ( 'NONE', #14041, 1000.000000000000000 ) ;
#10540 = DIRECTION ( 'NONE',  ( 1.734723475976809806E-16, -1.000000000000000000, 0.000000000000000000 ) ) ;
#10541 = VECTOR ( 'NONE', #14487, 1000.000000000000000 ) ;
#10542 = CARTESIAN_POINT ( 'NONE',  ( 1.021156010535390068, -3.846052534792979927, 2.579625955254269964 ) ) ;
#10543 = CIRCLE ( 'NONE', #16770, 0.04999999999999991257 ) ;
#10544 = CARTESIAN_POINT ( 'NONE',  ( 1.538437905834991515, -2.378890372630820149, 3.340547664492009350 ) ) ;
#10545 = EDGE_CURVE ( 'NONE', #16759, #16005, #2978, .T. ) ;
#10546 = LINE ( 'NONE', #14822, #9079 ) ;
#10547 = VECTOR ( 'NONE', #10435, 1000.000000000000000 ) ;
#10548 = AXIS2_PLACEMENT_3D ( 'NONE', #11220, #16680, #15406 ) ;
#10549 = LINE ( 'NONE', #14627, #1176 ) ;
#10550 = ORIENTED_EDGE ( 'NONE', *, *, #8237, .T. ) ;
#10551 = CARTESIAN_POINT ( 'NONE',  ( 1.585619829032530070, -0.5482184015263239507, 3.126197263413850180 ) ) ;
#10552 = LINE ( 'NONE', #9166, #7813 ) ;
#10553 = CARTESIAN_POINT ( 'NONE',  ( 1.214457691475989920, -3.869340823081270031, 2.684103622926340194 ) ) ;
#10554 = ORIENTED_EDGE ( 'NONE', *, *, #4156, .F. ) ;
#10555 = VERTEX_POINT ( 'NONE', #5660 ) ;
#10556 = LINE ( 'NONE', #10380, #17966 ) ;
#10557 = VECTOR ( 'NONE', #17523, 1000.000000000000000 ) ;
#10558 = ORIENTED_EDGE ( 'NONE', *, *, #1573, .F. ) ;
#10559 = CIRCLE ( 'NONE', #3186, 0.2000000000000000389 ) ;
#10560 = CARTESIAN_POINT ( 'NONE',  ( -2.329383452786330189, -4.571830348089889640, 5.035735636132877779 ) ) ;
#10561 = CONTEXT_DEPENDENT_SHAPE_REPRESENTATION ( #5203, #2074 ) ;
#10562 = CARTESIAN_POINT ( 'NONE',  ( -2.340070819011249803, -5.219915254237290192, 4.950151441910549899 ) ) ;
#10563 = DIRECTION ( 'NONE',  ( -7.109522442527898025E-16, 0.000000000000000000, -1.000000000000000000 ) ) ;
#10564 = CARTESIAN_POINT ( 'NONE',  ( 2.180207327701309872, -0.3934322033898309812, 5.586116916730190063 ) ) ;
#10565 = ORIENTED_EDGE ( 'NONE', *, *, #12243, .F. ) ;
#10566 = AXIS2_PLACEMENT_3D ( 'NONE', #17483, #12143, #17563 ) ;
#10567 = LINE ( 'NONE', #9179, #547 ) ;
#10568 = DIRECTION ( 'NONE',  ( 1.224646799147350002E-16, -1.000000000000000000, -6.123233995736769734E-17 ) ) ;
#10569 = CARTESIAN_POINT ( 'NONE',  ( -1.124021676335500208, -3.589881363621813648, 2.982013645643241340 ) ) ;
#10570 = EDGE_CURVE ( 'NONE', #10292, #13656, #9729, .T. ) ;
#10571 = CARTESIAN_POINT ( 'NONE',  ( 2.614198783383141045, -0.06673728813559372253, 4.243032045539284702 ) ) ;
#10572 = AXIS2_PLACEMENT_3D ( 'NONE', #10902, #12003, #13390 ) ;
#10573 = EDGE_LOOP ( 'NONE', ( #9169, #12078, #10776, #706 ) ) ;
#10574 = DIRECTION ( 'NONE',  ( 1.000000000000000000, 0.000000000000000000, 0.000000000000000000 ) ) ;
#10575 = CARTESIAN_POINT ( 'NONE',  ( 1.248294325655350034, -0.3266949152542379942, 2.704938983774300088 ) ) ;
#10576 = ORIENTED_EDGE ( 'NONE', *, *, #17183, .F. ) ;
#10577 = CARTESIAN_POINT ( 'NONE',  ( 0.7322514394120266390, -0.01334745762711889508, 2.149183891723918993 ) ) ;
#10578 = ORIENTED_EDGE ( 'NONE', *, *, #5415, .F. ) ;
#10579 = CARTESIAN_POINT ( 'NONE',  ( -1.248294325655370018, -5.573305084745760141, 2.704938983774309857 ) ) ;
#10580 = LINE ( 'NONE', #15400, #4675 ) ;
#10581 = VECTOR ( 'NONE', #11193, 1000.000000000000000 ) ;
#10582 = CARTESIAN_POINT ( 'NONE',  ( -1.571912189623050127, -1.264893411152959501, 6.451524409078660760 ) ) ;
#10583 = EDGE_CURVE ( 'NONE', #14447, #1528, #2693, .T. ) ;
#10584 = CARTESIAN_POINT ( 'NONE',  ( 1.925796468768800063, -5.404237288135590234, 6.052706598917719560 ) ) ;
#10585 = CARTESIAN_POINT ( 'NONE',  ( 1.373536515609961484, -4.381683165423609694, 6.970795264502707589 ) ) ;
#10586 = ORIENTED_EDGE ( 'NONE', *, *, #6878, .T. ) ;
#10587 = CARTESIAN_POINT ( 'NONE',  ( -0.1654173910288039839, -5.280843314568230085, 2.650679959339568459 ) ) ;
#10588 = CARTESIAN_POINT ( 'NONE',  ( 1.236334101859160040, -3.570433951693499974, 2.697445712080689617 ) ) ;
#10589 = DIRECTION ( 'NONE',  ( 1.000000000000000000, 0.000000000000000000, -7.401486830834380223E-16 ) ) ;
#10590 = FACE_OUTER_BOUND ( 'NONE', #12647, .T. ) ;
#10591 = VECTOR ( 'NONE', #10147, 1000.000000000000000 ) ;
#10592 = CARTESIAN_POINT ( 'NONE',  ( 1.616473591439308688, -3.989623140882693875, 5.965667796385536903 ) ) ;
#10593 = AXIS2_PLACEMENT_3D ( 'NONE', #1589, #4346, #4442 ) ;
#10594 = DIRECTION ( 'NONE',  ( 0.000000000000000000, 0.000000000000000000, 1.000000000000000000 ) ) ;
#10595 = PLANE ( 'NONE',  #7081 ) ;
#10596 = CARTESIAN_POINT ( 'NONE',  ( 1.423520578776751533, -2.056695212954759100, 3.220645071516909930 ) ) ;
#10597 = ORIENTED_EDGE ( 'NONE', *, *, #12698, .F. ) ;
#10598 = DIRECTION ( 'NONE',  ( -1.480297366166879989E-15, -2.476791224480699852E-30, -1.000000000000000000 ) ) ;
#10599 = AXIS2_PLACEMENT_3D ( 'NONE', #8908, #4638, #17221 ) ;
#10600 = EDGE_CURVE ( 'NONE', #2787, #6171, #7226, .T. ) ;
#10601 = CARTESIAN_POINT ( 'NONE',  ( 1.475946938622679783, -0.7471169921413568504, 2.482078242844649729 ) ) ;
#10602 = CARTESIAN_POINT ( 'NONE',  ( -2.550815101416269659, -1.404623140882690580, 5.432431574543720387 ) ) ;
#10603 = ORIENTED_EDGE ( 'NONE', *, *, #2719, .T. ) ;
#10604 = FACE_OUTER_BOUND ( 'NONE', #164, .T. ) ;
#10605 = LINE ( 'NONE', #11130, #10440 ) ;
#10606 = EDGE_CURVE ( 'NONE', #6296, #4438, #8345, .T. ) ;
#10607 = CYLINDRICAL_SURFACE ( 'NONE', #8589, 0.2500000000000002220 ) ;
#10608 = CARTESIAN_POINT ( 'NONE',  ( -1.750316316486840051, -5.259957627118650336, 3.126818518378589928 ) ) ;
#10609 = ORIENTED_EDGE ( 'NONE', *, *, #13294, .T. ) ;
#10610 = EDGE_CURVE ( 'NONE', #15567, #6801, #1493, .T. ) ;
#10611 = ORIENTED_EDGE ( 'NONE', *, *, #17839, .F. ) ;
#10612 = DIRECTION ( 'NONE',  ( -3.700743415417195042E-15, -3.289549702593060375E-15, 1.000000000000000000 ) ) ;
#10613 = EDGE_CURVE ( 'NONE', #2304, #5170, #16855, .T. ) ;
#10614 = CARTESIAN_POINT ( 'NONE',  ( -0.1749999999999999889, 6.799999999999999822, 0.5999999999999999778 ) ) ;
#10615 = VECTOR ( 'NONE', #6160, 1000.000000000000000 ) ;
#10616 = LINE ( 'NONE', #16265, #4625 ) ;
#10617 = ORIENTED_EDGE ( 'NONE', *, *, #1720, .F. ) ;
#10618 = CARTESIAN_POINT ( 'NONE',  ( -1.980638384804660257, -5.537711864406785978, 4.159858630563765480 ) ) ;
#10619 = EDGE_CURVE ( 'NONE', #1479, #305, #6943, .T. ) ;
#10620 = CARTESIAN_POINT ( 'NONE',  ( -1.428323476796611535, -3.290974492234041815, 2.463260019887531627 ) ) ;
#10621 = CARTESIAN_POINT ( 'NONE',  ( 0.5843165771433389555, -0.3612150962701970447, 2.403837883145311327 ) ) ;
#10622 = CARTESIAN_POINT ( 'NONE',  ( 2.398725280367429047, -2.448755237495690462, 3.564557036955152913 ) ) ;
#10623 = PRODUCT_DEFINITION_FORMATION_WITH_SPECIFIED_SOURCE ( 'ANY', '', #12599, .NOT_KNOWN. ) ;
#10624 = DIRECTION ( 'NONE',  ( 1.110223024625159992E-16, 0.000000000000000000, -1.000000000000000000 ) ) ;
#10625 = CARTESIAN_POINT ( 'NONE',  ( 3.673940397442059498E-17, 2.600000000000000089, 8.000000000000000000 ) ) ;
#10626 = CARTESIAN_POINT ( 'NONE',  ( 0.5902886515193200845, -4.152641158900699736, 6.978224088050040130 ) ) ;
#10627 = PLANE ( 'NONE',  #17049 ) ;
#10628 = DIRECTION ( 'NONE',  ( 0.000000000000000000, -1.000000000000000000, 0.000000000000000000 ) ) ;
#10630 = ORIENTED_EDGE ( 'NONE', *, *, #8622, .T. ) ;
#10629 = CARTESIAN_POINT ( 'NONE',  ( 1.720450724489989813, -2.774791273531719060, 6.720683794561567836 ) ) ;
#10631 = VECTOR ( 'NONE', #12891, 1000.000000000000227 ) ;
#10632 = CARTESIAN_POINT ( 'NONE',  ( 0.1749999999999999889, 8.800000000000000711, -3.200000000000000178 ) ) ;
#10633 = CARTESIAN_POINT ( 'NONE',  ( 0.2189795514005130062, -0.3044491525423729805, 2.356806637999009801 ) ) ;
#10634 = CARTESIAN_POINT ( 'NONE',  ( -1.381042549632419902, -1.540511994252449890, 6.605640880016140137 ) ) ;
#10635 = CARTESIAN_POINT ( 'NONE',  ( -2.155845792290839835, -0.5447033898305089217, 3.756158857535780271 ) ) ;
#10636 = CARTESIAN_POINT ( 'NONE',  ( -1.494590226124049792, -0.2673043920988010802, 2.870965838437660622 ) ) ;
#10637 = CARTESIAN_POINT ( 'NONE',  ( 2.519547246525509543, -5.359745762711870753, 3.866491354109194756 ) ) ;
#10638 = ORIENTED_EDGE ( 'NONE', *, *, #11485, .F. ) ;
#10639 = EDGE_CURVE ( 'NONE', #15319, #15809, #5564, .T. ) ;
#10640 = CARTESIAN_POINT ( 'NONE',  ( -0.9499999999999999556, 2.299999999999999822, 7.599999999999999645 ) ) ;
#10641 = ORIENTED_EDGE ( 'NONE', *, *, #12721, .T. ) ;
#10642 = CARTESIAN_POINT ( 'NONE',  ( 2.286166334984490067, -5.086440677966098889, 5.258525443163859059 ) ) ;
#10643 = CARTESIAN_POINT ( 'NONE',  ( -1.599999999999880185, 11.40000000000000036, 1.600000000000000089 ) ) ;
#10644 = CARTESIAN_POINT ( 'NONE',  ( 1.149999999999999911, 9.248236190979499227, 7.693185165257809821 ) ) ;
#10645 = APPLICATION_CONTEXT ( 'automotive_design' ) ;
#10646 = VERTEX_POINT ( 'NONE', #182 ) ;
#10647 = VECTOR ( 'NONE', #9142, 1000.000000000000000 ) ;
#10648 = ORIENTED_EDGE ( 'NONE', *, *, #17463, .T. ) ;
#10649 = CARTESIAN_POINT ( 'NONE',  ( -0.4201920264140019956, -2.122719201459649874, 2.384360920086639801 ) ) ;
#10650 = LINE ( 'NONE', #3601, #3190 ) ;
#10651 = CARTESIAN_POINT ( 'NONE',  ( 1.477796163681079911, -5.417584745762709986, 6.531563725478140015 ) ) ;
#10652 = CARTESIAN_POINT ( 'NONE',  ( 0.7678268402137939930, -2.867944426684879922, 6.924676972266129660 ) ) ;
#10653 = CARTESIAN_POINT ( 'NONE',  ( -1.286937324407759986, -3.589881363621809651, 2.729584305145209999 ) ) ;
#10654 = CARTESIAN_POINT ( 'NONE',  ( 2.048006021857541548, -2.541908390648840665, 4.556566471620634218 ) ) ;
#10655 = DIRECTION ( 'NONE',  ( 0.000000000000000000, -0.2588190451025180749, 0.9659258262890690894 ) ) ;
#10656 = VECTOR ( 'NONE', #5052, 1000.000000000000000 ) ;
#10657 = CARTESIAN_POINT ( 'NONE',  ( 0.07299321914061039640, -0.3014830508474579673, 2.350000000000000089 ) ) ;
#10658 = CARTESIAN_POINT ( 'NONE',  ( -1.550000000000000044, -6.000000000000000000, 6.100000000000000533 ) ) ;
#10659 = ORIENTED_EDGE ( 'NONE', *, *, #2642, .T. ) ;
#10660 = ADVANCED_FACE ( 'NONE', ( #15747 ), #11210, .F. ) ;
#10661 = CARTESIAN_POINT ( 'NONE',  ( 2.500000000000000000, 9.199999999999999289, 1.600000000000000089 ) ) ;
#10662 = CARTESIAN_POINT ( 'NONE',  ( 1.724579595320000047, -3.939205687946140344, 3.098572228637889836 ) ) ;
#10663 = ORIENTED_EDGE ( 'NONE', *, *, #215, .F. ) ;
#10664 = ORIENTED_EDGE ( 'NONE', *, *, #1049, .T. ) ;
#10665 = DIRECTION ( 'NONE',  ( 0.000000000000000000, -1.000000000000000000, 0.000000000000000000 ) ) ;
#10666 = ORIENTED_EDGE ( 'NONE', *, *, #5956, .F. ) ;
#10667 = LINE ( 'NONE', #5105, #15127 ) ;
#10668 = PRODUCT_CONTEXT ( 'NONE', #10645, 'mechanical' ) ;
#10669 = CARTESIAN_POINT ( 'NONE',  ( -0.4917262214559124933, -5.291101694915254505, 2.092115739186370948 ) ) ;
#10670 = PRODUCT_DEFINITION_SHAPE ( 'NONE', 'NONE',  #15932 ) ;
#10671 = AXIS2_PLACEMENT_3D ( 'NONE', #12105, #17904, #15165 ) ;
#10672 = FACE_OUTER_BOUND ( 'NONE', #7120, .T. ) ;
#10673 = DIRECTION ( 'NONE',  ( 1.000000000000000000, 0.000000000000000000, 0.000000000000000000 ) ) ;
#10674 = DIRECTION ( 'NONE',  ( 1.000000000000000000, 1.908195823574489776E-16, 1.110223024625159992E-16 ) ) ;
#10675 = CARTESIAN_POINT ( 'NONE',  ( 1.831349212334668852, -4.009070552811004440, 3.772065786216904026 ) ) ;
#10676 = CARTESIAN_POINT ( 'NONE',  ( -1.873832970144350130, -0.5625000000000005551, 2.826167029855650270 ) ) ;
#10677 = ORIENTED_EDGE ( 'NONE', *, *, #9002, .T. ) ;
#10678 = CARTESIAN_POINT ( 'NONE',  ( 2.270487904532159984, -0.3622881355932209835, 4.080813552109670894 ) ) ;
#10679 = CARTESIAN_POINT ( 'NONE',  ( 0.07299321914061039640, -0.001483050847457899942, 2.350000000000000089 ) ) ;
#10680 = ORIENTED_EDGE ( 'NONE', *, *, #17162, .T. ) ;
#10681 = CARTESIAN_POINT ( 'NONE',  ( 0.1749999999999999889, 8.200000000000001066, 0.4000000000000000222 ) ) ;
#10682 = CARTESIAN_POINT ( 'NONE',  ( -0.7983658734557950165, -5.466525423728810118, 6.913847129767330735 ) ) ;
#10683 = CARTESIAN_POINT ( 'NONE',  ( -1.000000000000000000, -8.000000000000000000, 3.700000000000000178 ) ) ;
#10684 = LINE ( 'NONE', #10869, #10983 ) ;
#10685 = CARTESIAN_POINT ( 'NONE',  ( 2.286166334984490067, -5.386440677966100488, 5.258525443163859947 ) ) ;
#10686 = CARTESIAN_POINT ( 'NONE',  ( -1.447263454062130528, -4.661142624883069630, 6.924531903016462486 ) ) ;
#10687 = ORIENTED_EDGE ( 'NONE', *, *, #6329, .T. ) ;
#10688 = CARTESIAN_POINT ( 'NONE',  ( -0.1881942810071039751, -5.280843314568230085, 2.350674491507239949 ) ) ;
#10689 = CARTESIAN_POINT ( 'NONE',  ( 2.353343516942209668, -3.826605122864669806, 4.722803042560139275 ) ) ;
#10690 = CARTESIAN_POINT ( 'NONE',  ( -2.006003143955999324, -4.731007489747939054, 6.437545705712661714 ) ) ;
#10691 = LINE ( 'NONE', #6518, #18194 ) ;
#10692 = DIRECTION ( 'NONE',  ( -0.7071067811865480168, 0.7071067811865470176, 0.000000000000000000 ) ) ;
#10693 = CARTESIAN_POINT ( 'NONE',  ( 0.1781895581254300809, -3.453992510252061887, 2.654724878163539969 ) ) ;
#10694 = DIRECTION ( 'NONE',  ( 1.000000000000000000, 1.233581138472399909E-16, 1.480297366166879989E-16 ) ) ;
#10695 = DIRECTION ( 'NONE',  ( -1.000000000000000000, 0.000000000000000000, 0.000000000000000000 ) ) ;
#10696 = CARTESIAN_POINT ( 'NONE',  ( -2.016543577558690625, -1.521064582324129777, 4.314702916654059806 ) ) ;
#10697 = ORIENTED_EDGE ( 'NONE', *, *, #15271, .F. ) ;
#10698 = DIRECTION ( 'NONE',  ( 0.000000000000000000, 0.8944271909999159664, -0.4472135954999579832 ) ) ;
#10699 = CARTESIAN_POINT ( 'NONE',  ( -1.899999999999999911, 9.199999999999999289, 1.600000000000000089 ) ) ;
#10700 = CARTESIAN_POINT ( 'NONE',  ( 0.6575972843460591299, -0.3612150962701959900, 2.110392115010549130 ) ) ;
#10701 = CARTESIAN_POINT ( 'NONE',  ( 2.574214976178930137, -2.196424942684489956, 4.054607910322744146 ) ) ;
#10702 = ORIENTED_EDGE ( 'NONE', *, *, #8688, .T. ) ;
#10703 = CARTESIAN_POINT ( 'NONE',  ( 2.500000000000000000, 3.500000000000000000, 0.6099999999999999867 ) ) ;
#10704 = CARTESIAN_POINT ( 'NONE',  ( -1.003115764947269950, -1.493935417675869903, 6.828967930617589666 ) ) ;
#10705 = CARTESIAN_POINT ( 'NONE',  ( -2.116444151961480280, -5.246610169491529696, 3.670839500609359707 ) ) ;
#10706 = VERTEX_POINT ( 'NONE', #10524 ) ;
#10707 = ORIENTED_EDGE ( 'NONE', *, *, #6657, .F. ) ;
#10708 = PLANE ( 'NONE',  #10671 ) ;
#10709 = DIRECTION ( 'NONE',  ( 1.000000000000000000, 1.224646799147350002E-16, 0.000000000000000000 ) ) ;
#10710 = DIRECTION ( 'NONE',  ( -1.000000000000000000, 0.000000000000000000, 6.123233995736769734E-17 ) ) ;
#10711 = CARTESIAN_POINT ( 'NONE',  ( -1.549742865090599997, -5.484322033898309634, 6.471102547561460305 ) ) ;
#10712 = CARTESIAN_POINT ( 'NONE',  ( 2.623186471072028514, -2.219713230972778728, 4.297499775172036962 ) ) ;
#10713 = DIRECTION ( 'NONE',  ( 1.000000000000000000, 0.000000000000000000, 0.000000000000000000 ) ) ;
#10714 = PLANE ( 'NONE',  #8524 ) ;
#10715 = DIRECTION ( 'NONE',  ( 6.123233995736806712E-17, 0.000000000000000000, 1.000000000000000000 ) ) ;
#10716 = CARTESIAN_POINT ( 'NONE',  ( -0.4539185741479770386, -3.384127645387189798, 2.390735265170449875 ) ) ;
#10717 = ADVANCED_FACE ( 'NONE', ( #16099 ), #14611, .T. ) ;
#10718 = LINE ( 'NONE', #14790, #15887 ) ;
#10719 = CARTESIAN_POINT ( 'NONE',  ( -1.899999999999999911, 9.199999999999999289, 1.600000000000000089 ) ) ;
#10721 = ORIENTED_EDGE ( 'NONE', *, *, #2803, .F. ) ;
#10720 = CARTESIAN_POINT ( 'NONE',  ( 1.818868030982612183, -2.355602084342530933, 2.767428454397789839 ) ) ;
#10722 = EDGE_CURVE ( 'NONE', #2252, #2762, #7313, .T. ) ;
#10723 = EDGE_CURVE ( 'NONE', #17164, #13357, #13049, .T. ) ;
#10724 = CARTESIAN_POINT ( 'NONE',  ( -1.889999999999999902, 4.700000000000000178, -5.551115123125779744E-16 ) ) ;
#10725 = DIRECTION ( 'NONE',  ( -1.000000000000000000, 0.000000000000000000, 0.000000000000000000 ) ) ;
#10726 = CARTESIAN_POINT ( 'NONE',  ( -0.8001898266890440370, -1.470647129387580021, 6.913242401714570384 ) ) ;
#10727 = CARTESIAN_POINT ( 'NONE',  ( 2.200000000000000178, 1.815095292823759964E-16, 4.000000000000000000 ) ) ;
#10728 = DIRECTION ( 'NONE',  ( 1.000000000000000000, 0.000000000000000000, 0.000000000000000000 ) ) ;
#10729 = CARTESIAN_POINT ( 'NONE',  ( 2.650076489488250697, -5.377542372881360500, 4.841243018609314497 ) ) ;
#10730 = ORIENTED_EDGE ( 'NONE', *, *, #9489, .F. ) ;
#10731 = CARTESIAN_POINT ( 'NONE',  ( -0.9999999999999978906, 9.099999999999999645, 7.700000000000000178 ) ) ;
#10732 = EDGE_LOOP ( 'NONE', ( #2473, #3095, #13879, #10520, #6907, #15935, #9264, #8042 ) ) ;
#10733 = FACE_OUTER_BOUND ( 'NONE', #10120, .T. ) ;
#10734 = LINE ( 'NONE', #9333, #17974 ) ;
#10735 = ORIENTED_EDGE ( 'NONE', *, *, #11868, .F. ) ;
#10736 = CARTESIAN_POINT ( 'NONE',  ( -0.7435598031058080482, -3.030962444702889780, 6.932904947974540377 ) ) ;
#10737 = EDGE_CURVE ( 'NONE', #2948, #12005, #4518, .T. ) ;
#10738 = CARTESIAN_POINT ( 'NONE',  ( 0.1749999999999999889, 9.299999999999998934, 0.5999999999999999778 ) ) ;
#10739 = CARTESIAN_POINT ( 'NONE',  ( 0.9000000000000000222, -9.500000000000000000, 1.300000000000000044 ) ) ;
#10740 = LINE ( 'NONE', #12226, #6085 ) ;
#10741 = ADVANCED_FACE ( 'NONE', ( #16189 ), #1848, .T. ) ;
#10742 = CARTESIAN_POINT ( 'NONE',  ( 2.337178851518220135, -2.588484967225419986, 4.976298214796759822 ) ) ;
#10743 = FACE_OUTER_BOUND ( 'NONE', #15595, .T. ) ;
#10744 = CARTESIAN_POINT ( 'NONE',  ( -0.5549238885286955636, -2.099430913171361102, 2.723396519134838822 ) ) ;
#10745 = CARTESIAN_POINT ( 'NONE',  ( 1.149999999999999911, 6.472933199251450276, 6.846017351831609865 ) ) ;
#10746 = CARTESIAN_POINT ( 'NONE',  ( 1.057242234132090175, -0.3222457627118650025, 2.597442975781520058 ) ) ;
#10747 = CARTESIAN_POINT ( 'NONE',  ( -0.009452110982655708218, -0.5998079552954630467, 2.350000000000000089 ) ) ;
#10748 = ORIENTED_EDGE ( 'NONE', *, *, #4296, .T. ) ;
#10749 = CARTESIAN_POINT ( 'NONE',  ( 0.9000000000000000222, 2.050000000000000266, 1.600000000000000089 ) ) ;
#10750 = DIRECTION ( 'NONE',  ( -8.397698689135169229E-17, 1.000000000000000000, 0.000000000000000000 ) ) ;
#10751 = CARTESIAN_POINT ( 'NONE',  ( -0.4790341583531910197, -3.683034516774959855, 2.395814251711740006 ) ) ;
#10752 = ORIENTED_EDGE ( 'NONE', *, *, #14504, .F. ) ;
#10753 = EDGE_LOOP ( 'NONE', ( #13723, #183, #7392, #16083 ) ) ;
#10754 = DIRECTION ( 'NONE',  ( 0.000000000000000000, 0.000000000000000000, 1.000000000000000000 ) ) ;
#10755 = EDGE_LOOP ( 'NONE', ( #11309, #186 ) ) ;
#10756 = CARTESIAN_POINT ( 'NONE',  ( -2.231116159141639521, -4.688271789531330391, 3.951089877392499616 ) ) ;
#10757 = AXIS2_PLACEMENT_3D ( 'NONE', #629, #9323, #4786 ) ;
#10758 = ITEM_DEFINED_TRANSFORMATION ( 'NONE', 'NONE', #14162,  #17681 ) ;
#10759 = CARTESIAN_POINT ( 'NONE',  ( -2.180207327701300102, -5.206567796610169552, 5.586116916730199833 ) ) ;
#10760 = ADVANCED_FACE ( 'NONE', ( #17549 ), #14340, .F. ) ;
#10761 = DIRECTION ( 'NONE',  ( -0.000000000000000000, 1.000000000000000000, 0.000000000000000000 ) ) ;
#10762 = ORIENTED_EDGE ( 'NONE', *, *, #11912, .T. ) ;
#10763 = CARTESIAN_POINT ( 'NONE',  ( -2.342931736853879787, -1.497776294035840117, 4.477701633099189671 ) ) ;
#10764 = EDGE_CURVE ( 'NONE', #2515, #5242, #895, .T. ) ;
#10765 = PLANE ( 'NONE',  #10861 ) ;
#10766 = CARTESIAN_POINT ( 'NONE',  ( 0.7109160811436110450, -1.307629111369560171, 6.943511536198400336 ) ) ;
#10767 = CARTESIAN_POINT ( 'NONE',  ( 1.428515267734870031, -0.03114406779661050076, 2.829745655876919841 ) ) ;
#10768 = ORIENTED_EDGE ( 'NONE', *, *, #11513, .T. ) ;
#10769 = CIRCLE ( 'NONE', #1893, 0.3999999999999999667 ) ;
#10770 = CARTESIAN_POINT ( 'NONE',  ( 1.128670402850170174, -0.1290254237288140371, 7.101865548313628373 ) ) ;
#10771 = ORIENTED_EDGE ( 'NONE', *, *, #15271, .T. ) ;
#10772 = LINE ( 'NONE', #15421, #7075 ) ;
#10773 = DIRECTION ( 'NONE',  ( 4.898042755699219270E-17, -1.000000000000000000, 0.000000000000000000 ) ) ;
#10774 = CARTESIAN_POINT ( 'NONE',  ( 2.058670345754650022, -5.350847457627120107, 3.559656372813920111 ) ) ;
#10775 = CARTESIAN_POINT ( 'NONE',  ( 0.5355577887186364627, -1.032010528270079330, 7.299286738308158107 ) ) ;
#10776 = ORIENTED_EDGE ( 'NONE', *, *, #16148, .F. ) ;
#10777 = CARTESIAN_POINT ( 'NONE',  ( -0.1458667720079689645, -4.981295943764795453, 2.649245313618650677 ) ) ;
#10778 = CARTESIAN_POINT ( 'NONE',  ( -2.226511124464849889, -4.525253771513310319, 5.462491901673850236 ) ) ;
#10779 = CARTESIAN_POINT ( 'NONE',  ( -2.622715975066178817, -4.870737219477664581, 5.105554690683034913 ) ) ;
#10780 = EDGE_CURVE ( 'NONE', #18075, #14363, #5915, .T. ) ;
#10781 = CARTESIAN_POINT ( 'NONE',  ( -1.000000000000000000, 5.400000000000000355, 7.700000000000000178 ) ) ;
#10782 = PLANE ( 'NONE',  #5525 ) ;
#10783 = CARTESIAN_POINT ( 'NONE',  ( 0.5549238885286489342, -3.500569086828633658, 2.723396519134821059 ) ) ;
#10784 = DIRECTION ( 'NONE',  ( -1.224646799147351975E-16, 1.000000000000000000, 6.123233995736759873E-17 ) ) ;
#10785 = CARTESIAN_POINT ( 'NONE',  ( 0.5500000000000000444, 0.5999999999999999778, 3.299999999999999822 ) ) ;
#10786 = CARTESIAN_POINT ( 'NONE',  ( 0.6050872056802326648, -1.940253771513320125, 2.738171435586128410 ) ) ;
#10787 = ORIENTED_EDGE ( 'NONE', *, *, #10379, .T. ) ;
#10788 = DIRECTION ( 'NONE',  ( -1.000000000000000000, 0.000000000000000000, 0.000000000000000000 ) ) ;
#10789 = CARTESIAN_POINT ( 'NONE',  ( 1.889999999999999902, 3.500000000000000000, 0.6099999999999999867 ) ) ;
#10790 = CARTESIAN_POINT ( 'NONE',  ( 0.9724415447670879953, -0.7068739681193980662, 2.553509270169310064 ) ) ;
#10791 = CARTESIAN_POINT ( 'NONE',  ( -2.494165244384181079, -3.127956474216021299, 3.793218093085275910 ) ) ;
#10792 = EDGE_LOOP ( 'NONE', ( #14441, #700, #4286, #5059 ) ) ;
#10793 = LINE ( 'NONE', #11907, #8200 ) ;
#10794 = LINE ( 'NONE', #17615, #11539 ) ;
#10795 = CARTESIAN_POINT ( 'NONE',  ( 1.562863241354470523, -5.108686440677975504, 6.031217337312382298 ) ) ;
#10796 = ORIENTED_EDGE ( 'NONE', *, *, #12779, .T. ) ;
#10797 = EDGE_LOOP ( 'NONE', ( #17833, #9530, #10916, #1068 ) ) ;
#10798 = CARTESIAN_POINT ( 'NONE',  ( 0.6914213562373080491, 6.450000000000000178, 2.557842712474620139 ) ) ;
#10799 = FACE_OUTER_BOUND ( 'NONE', #18147, .T. ) ;
#10800 = EDGE_LOOP ( 'NONE', ( #10311, #17055, #7370, #17550 ) ) ;
#10801 = CARTESIAN_POINT ( 'NONE',  ( -1.851073041990159984, -5.493220338983049622, 6.153284478378270528 ) ) ;
#10802 = CARTESIAN_POINT ( 'NONE',  ( 2.218077401483169897, -0.7758393570989060573, 5.486688202856499608 ) ) ;
#10803 = CARTESIAN_POINT ( 'NONE',  ( -0.7999999999998790301, 11.40000000000000036, -9.797174393178840942E-17 ) ) ;
#10804 = CARTESIAN_POINT ( 'NONE',  ( -2.523518139275819916, -3.263845327585779277, 5.521565513971835593 ) ) ;
#10805 = CARTESIAN_POINT ( 'NONE',  ( -1.599999999999880185, 11.40000000000000036, 1.600000000000000089 ) ) ;
#10806 = LINE ( 'NONE', #12011, #237 ) ;
#10807 = CARTESIAN_POINT ( 'NONE',  ( -2.322440385110939864, -3.081379897639439758, 4.319189883157439347 ) ) ;
#10808 = FACE_OUTER_BOUND ( 'NONE', #4412, .T. ) ;
#10809 = LINE ( 'NONE', #3769, #16532 ) ;
#10811 = ORIENTED_EDGE ( 'NONE', *, *, #1802, .T. ) ;
#10810 = CARTESIAN_POINT ( 'NONE',  ( -0.9490039995899379743, -2.076142624883081211, 2.221592224478750488 ) ) ;
#10812 = LINE ( 'NONE', #11927, #15050 ) ;
#10813 = CARTESIAN_POINT ( 'NONE',  ( 1.750316316486830059, -0.3400423728813560253, 3.126818518378580158 ) ) ;
#10814 = CARTESIAN_POINT ( 'NONE',  ( -2.340959815966380031, -1.750106588847040179, 4.942183458383479611 ) ) ;
#10815 = CARTESIAN_POINT ( 'NONE',  ( 0.005141112625543309625, -5.068517718233539249, 2.221989741495029591 ) ) ;
#10816 = CARTESIAN_POINT ( 'NONE',  ( -0.3367924244280810497, 2.254758922476410188, 7.700000000000000178 ) ) ;
#10817 = VERTEX_POINT ( 'NONE', #630 ) ;
#10818 = PRODUCT_DEFINITION_SHAPE ( 'NONE', 'NONE',  #13304 ) ;
#10819 = SURFACE_SIDE_STYLE ('',( #13612 ) ) ;
#10820 = ORIENTED_EDGE ( 'NONE', *, *, #15715, .F. ) ;
#10821 = CARTESIAN_POINT ( 'NONE',  ( -0.3743405594629429789, -5.157627118644069419, 7.023440622744399953 ) ) ;
#10822 = PLANE ( 'NONE',  #766 ) ;
#10823 = DIRECTION ( 'NONE',  ( 0.000000000000000000, 0.000000000000000000, 1.000000000000000000 ) ) ;
#10824 = AXIS2_PLACEMENT_3D ( 'NONE', #6017, #2734, #8886 ) ;
#10825 = ADVANCED_FACE ( 'NONE', ( #11930 ), #14440, .T. ) ;
#10826 = VERTEX_POINT ( 'NONE', #6188 ) ;
#10827 = ADVANCED_FACE ( 'NONE', ( #1925 ), #4878, .T. ) ;
#10828 = CIRCLE ( 'NONE', #8463, 0.1499999999999999667 ) ;
#10829 = CARTESIAN_POINT ( 'NONE',  ( -1.630481553867809907, -3.543304787045240101, 3.002862530617889547 ) ) ;
#10830 = CARTESIAN_POINT ( 'NONE',  ( 2.500000000000000000, 8.500000000000000000, 0.6099999999999999867 ) ) ;
#10831 = DIRECTION ( 'NONE',  ( 1.306144734853129823E-16, -2.378183611328045350E-31, 1.000000000000000000 ) ) ;
#10832 = CARTESIAN_POINT ( 'NONE',  ( -1.750000000000000000, 11.40000000000000036, 7.599999999999999645 ) ) ;
#10833 = CARTESIAN_POINT ( 'NONE',  ( -1.332058588847369940, -3.100827309567760537, 6.640197310420220767 ) ) ;
#10834 = DIRECTION ( 'NONE',  ( 1.000000000000000000, -2.220446049250309876E-16, -7.401486830834380223E-16 ) ) ;
#10835 = CARTESIAN_POINT ( 'NONE',  ( 0.2047443300700049207, -2.192584066324520187, 2.657212296411530783 ) ) ;
#10836 = VECTOR ( 'NONE', #17229, 1000.000000000000114 ) ;
#10837 = PLANE ( 'NONE',  #15035 ) ;
#10838 = CARTESIAN_POINT ( 'NONE',  ( -1.494590226124050014, -0.2673043920988010247, 2.870965838437660178 ) ) ;
#10839 = ORIENTED_EDGE ( 'NONE', *, *, #2035, .T. ) ;
#10840 = CARTESIAN_POINT ( 'NONE',  ( -0.1749999999999999889, 7.700000000000000178, 1.600000000000000089 ) ) ;
#10841 = EDGE_CURVE ( 'NONE', #9046, #11652, #11845, .T. ) ;
#10842 = CARTESIAN_POINT ( 'NONE',  ( -1.149999999999999911, 9.299999999999998934, 7.700000000000000178 ) ) ;
#10843 = FILL_AREA_STYLE ('',( #13633 ) ) ;
#10844 = ORIENTED_EDGE ( 'NONE', *, *, #15142, .F. ) ;
#10845 = ORIENTED_EDGE ( 'NONE', *, *, #5048, .F. ) ;
#10846 = EDGE_CURVE ( 'NONE', #14829, #12759, #17382, .T. ) ;
#10847 = UNCERTAINTY_MEASURE_WITH_UNIT (LENGTH_MEASURE( 1.000000000000000082E-05 ), #5546, 'distance_accuracy_value', 'NONE');
#10848 = EDGE_CURVE ( 'NONE', #17593, #14634, #11823, .T. ) ;
#10849 = VERTEX_POINT ( 'NONE', #8877 ) ;
#10850 = CARTESIAN_POINT ( 'NONE',  ( 0.1749999999999999889, 5.200000000000000178, 1.600000000000000089 ) ) ;
#10851 = ADVANCED_FACE ( 'NONE', ( #14527 ), #6093, .F. ) ;
#10852 = CARTESIAN_POINT ( 'NONE',  ( 1.641808337277750107, -5.113135593220339281, 6.386111670537619744 ) ) ;
#10853 = EDGE_CURVE ( 'NONE', #5435, #3235, #4702, .T. ) ;
#10854 = VECTOR ( 'NONE', #15662, 1000.000000000000000 ) ;
#10855 = DIRECTION ( 'NONE',  ( 0.000000000000000000, -1.000000000000000000, 0.000000000000000000 ) ) ;
#10856 = AXIS2_PLACEMENT_3D ( 'NONE', #17527, #16160, #9113 ) ;
#10857 = EDGE_LOOP ( 'NONE', ( #219, #5877, #11963, #4350, #210, #2394 ) ) ;
#10858 = CARTESIAN_POINT ( 'NONE',  ( 0.8934014991060330590, -0.9854339516935011201, 6.877287176483390496 ) ) ;
#10859 = CARTESIAN_POINT ( 'NONE',  ( -1.661700935788390066, -4.954166666666670160, 3.038299064211620326 ) ) ;
#10860 = CARTESIAN_POINT ( 'NONE',  ( -0.8001898266890440370, -1.470647129387580021, 6.913242401714570384 ) ) ;
#10861 = AXIS2_PLACEMENT_3D ( 'NONE', #7998, #9365, #13730 ) ;
#10862 = VECTOR ( 'NONE', #2758, 1000.000000000000000 ) ;
#10863 = CARTESIAN_POINT ( 'NONE',  ( -2.650076489488250697, -0.2224576271186441134, 4.841243018609314497 ) ) ;
#10864 = CARTESIAN_POINT ( 'NONE',  ( -2.234315482767910144, -0.5402542372881360411, 3.960850823455329905 ) ) ;
#10865 = VECTOR ( 'NONE', #9863, 1000.000000000000000 ) ;
#10866 = EDGE_LOOP ( 'NONE', ( #16874, #141, #15223, #3309 ) ) ;
#10867 = FACE_OUTER_BOUND ( 'NONE', #17313, .T. ) ;
#10868 = EDGE_CURVE ( 'NONE', #12508, #13175, #11666, .T. ) ;
#10869 = CARTESIAN_POINT ( 'NONE',  ( 2.500000000000000000, 10.00000000000000000, 1.600000000000000089 ) ) ;
#10870 = CARTESIAN_POINT ( 'NONE',  ( -1.221947981261169991, -0.5741044150835520332, 2.670403636935529956 ) ) ;
#10871 = VECTOR ( 'NONE', #297, 1000.000000000000000 ) ;
#10872 = AXIS2_PLACEMENT_3D ( 'NONE', #10303, #2050, #10563 ) ;
#10873 = VECTOR ( 'NONE', #16184, 1000.000000000000000 ) ;
#10874 = CARTESIAN_POINT ( 'NONE',  ( 2.573461662271340877, -0.7525510688106187285, 5.348389362822485893 ) ) ;
#10875 = ORIENTED_EDGE ( 'NONE', *, *, #12357, .T. ) ;
#10876 = CARTESIAN_POINT ( 'NONE',  ( 0.9499999999999999556, 2.299999999999999822, 7.599999999999999645 ) ) ;
#10877 = CARTESIAN_POINT ( 'NONE',  ( 1.197297565406180153, -4.082776294035840969, 6.726135293448179731 ) ) ;
#10878 = VECTOR ( 'NONE', #16264, 1000.000000000000000 ) ;
#10879 = DIRECTION ( 'NONE',  ( 0.000000000000000000, -8.217301096052200103E-32, -1.000000000000000000 ) ) ;
#10880 = CARTESIAN_POINT ( 'NONE',  ( -1.942813984510721070, -4.525253771513313872, 5.363608065214459764 ) ) ;
#10881 = CYLINDRICAL_SURFACE ( 'NONE', #10272, 0.1000000000000000472 ) ;
#10882 = CARTESIAN_POINT ( 'NONE',  ( -1.000000000000000000, -5.599999999999999645, 5.100000000000000533 ) ) ;
#10883 = ADVANCED_FACE ( 'NONE', ( #16567 ), #10922, .F. ) ;
#10884 = CARTESIAN_POINT ( 'NONE',  ( -0.2047443300700520219, -3.407415933675483899, 2.657212296411530783 ) ) ;
#10885 = EDGE_LOOP ( 'NONE', ( #17195, #10103, #5315, #16345 ) ) ;
#10886 = CARTESIAN_POINT ( 'NONE',  ( -1.889999999999999902, 4.700000000000000178, 0.6099999999999999867 ) ) ;
#10887 = DIRECTION ( 'NONE',  ( -1.000000000000000000, 0.000000000000000000, 0.000000000000000000 ) ) ;
#10888 = VECTOR ( 'NONE', #4996, 1000.000000000000000 ) ;
#10889 = CARTESIAN_POINT ( 'NONE',  ( -1.880631435828179265, -0.2447033898305090438, 3.876649216148230437 ) ) ;
#10890 = APPLICATION_CONTEXT ( 'automotive_design' ) ;
#10891 = AXIS2_PLACEMENT_3D ( 'NONE', #16936, #7148, #12957 ) ;
#10892 = CARTESIAN_POINT ( 'NONE',  ( 0.6370285429020036139, -0.6606104644819236205, 2.105399314608770833 ) ) ;
#10893 = CARTESIAN_POINT ( 'NONE',  ( 1.837442528958791010, -2.056695212954759100, 2.785079989718789673 ) ) ;
#10894 = DIRECTION ( 'NONE',  ( -1.000000000000000000, 0.000000000000000000, 0.000000000000000000 ) ) ;
#10895 = CARTESIAN_POINT ( 'NONE',  ( -6.735557395310440051E-17, 7.000000000000000000, 6.299999999999999822 ) ) ;
#10896 = CARTESIAN_POINT ( 'NONE',  ( 1.134881315981519645, -5.122033898305085486, 6.410767520434657918 ) ) ;
#10897 = ORIENTED_EDGE ( 'NONE', *, *, #7682, .F. ) ;
#10898 = EDGE_CURVE ( 'NONE', #11273, #13665, #2210, .T. ) ;
#10899 = AXIS2_PLACEMENT_3D ( 'NONE', #1791, #9849, #7435 ) ;
#10900 = EDGE_LOOP ( 'NONE', ( #5958, #11282, #4312, #2957 ) ) ;
#10901 = FACE_OUTER_BOUND ( 'NONE', #15963, .T. ) ;
#10902 = CARTESIAN_POINT ( 'NONE',  ( 4.898587196589409994E-17, 0.1000000000000000056, 8.300000000000000711 ) ) ;
#10903 = SPHERICAL_SURFACE ( 'NONE', #13818, 1.100000000000000089 ) ;
#10904 = EDGE_LOOP ( 'NONE', ( #4738, #7708, #11795, #3811 ) ) ;
#10905 = CARTESIAN_POINT ( 'NONE',  ( -2.345900685764729765, -5.528813559322030002, 4.512231114381339836 ) ) ;
#10906 = VECTOR ( 'NONE', #17955, 1000.000000000000000 ) ;
#10907 = VECTOR ( 'NONE', #2982, 1000.000000000000000 ) ;
#10908 = CARTESIAN_POINT ( 'NONE',  ( 2.653777292528160192, -3.826605122864674247, 4.724078510415155030 ) ) ;
#10909 = CARTESIAN_POINT ( 'NONE',  ( 1.670747152266691016, -0.4963810343603142217, 3.047345280935851441 ) ) ;
#10910 = CARTESIAN_POINT ( 'NONE',  ( -1.011820239713360658, -3.636457940198391636, 2.246566997958110434 ) ) ;
#10911 = DIRECTION ( 'NONE',  ( 0.000000000000000000, 1.000000000000000000, 2.220446049250309876E-16 ) ) ;
#10912 = CARTESIAN_POINT ( 'NONE',  ( -0.1608173401625278554, -1.101875393134940984, 6.746714348835997299 ) ) ;
#10913 = PLANE ( 'NONE',  #7901 ) ;
#10914 = DIRECTION ( 'NONE',  ( 1.000000000000000000, -1.224646799147350002E-16, 0.000000000000000000 ) ) ;
#10916 = ORIENTED_EDGE ( 'NONE', *, *, #14700, .F. ) ;
#10915 = CARTESIAN_POINT ( 'NONE',  ( -0.7137241095604881513, -2.099430913171361102, 2.143887406933340678 ) ) ;
#10917 = CARTESIAN_POINT ( 'NONE',  ( -1.550000000000000044, -5.599999999999999645, 5.100000000000000533 ) ) ;
#10918 = CARTESIAN_POINT ( 'NONE',  ( -1.300961508564169922, -0.4779661016949160457, 6.661123742937279602 ) ) ;
#10919 = CIRCLE ( 'NONE', #13270, 0.1000000000000000472 ) ;
#10920 = CARTESIAN_POINT ( 'NONE',  ( 1.074829861819710075, -2.285737219477669946, 2.606322265575589991 ) ) ;
#10921 = CARTESIAN_POINT ( 'NONE',  ( -1.713314936023349944, -0.5610169491525430763, 3.089913064446579760 ) ) ;
#10922 = CYLINDRICAL_SURFACE ( 'NONE', #8579, 0.1000000000000001443 ) ;
#10923 = CARTESIAN_POINT ( 'NONE',  ( -2.458531667407850563, -5.506567796610171150, 5.699238225248945966 ) ) ;
#10924 = ORIENTED_EDGE ( 'NONE', *, *, #1802, .F. ) ;
#10925 = DIRECTION ( 'NONE',  ( 7.401486830834380223E-16, -8.540177112501229283E-17, 1.000000000000000000 ) ) ;
#10926 = CARTESIAN_POINT ( 'NONE',  ( 1.300961508564179692, -5.122033898305089039, 6.661123742937278713 ) ) ;
#10927 = DIRECTION ( 'NONE',  ( 0.000000000000000000, 0.000000000000000000, -1.000000000000000000 ) ) ;
#10928 = DIRECTION ( 'NONE',  ( 0.000000000000000000, 0.000000000000000000, 1.000000000000000000 ) ) ;
#10929 = EDGE_LOOP ( 'NONE', ( #17278, #859, #9212, #8856 ) ) ;
#10930 = CARTESIAN_POINT ( 'NONE',  ( -0.4735094604798580353, -4.567989471729919870, 7.005327412390699671 ) ) ;
#10931 = CARTESIAN_POINT ( 'NONE',  ( -2.253200202764409799, -5.511016949152540256, 5.379408587037509903 ) ) ;
#10932 = VECTOR ( 'NONE', #4366, 1000.000000000000000 ) ;
#10933 = DIRECTION ( 'NONE',  ( 0.000000000000000000, 0.000000000000000000, 1.000000000000000000 ) ) ;
#10934 = DIRECTION ( 'NONE',  ( -0.000000000000000000, 1.000000000000000000, 0.000000000000000000 ) ) ;
#10935 = CARTESIAN_POINT ( 'NONE',  ( -0.9485663501270049647, -3.054250732991179440, 6.853826262002260528 ) ) ;
#10936 = PLANE ( 'NONE',  #13179 ) ;
#10937 = CARTESIAN_POINT ( 'NONE',  ( -1.919159680931840084, -1.866548030288480042, 3.970803207828165426 ) ) ;
#10938 = CARTESIAN_POINT ( 'NONE',  ( -0.7093417302541390468, -0.4646186440677970153, 6.943956659919700236 ) ) ;
#10939 = FACE_OUTER_BOUND ( 'NONE', #4373, .T. ) ;
#10940 = ADVANCED_FACE ( 'NONE', ( #3874 ), #5165, .T. ) ;
#10941 = PLANE ( 'NONE',  #572 ) ;
#10942 = VERTEX_POINT ( 'NONE', #10816 ) ;
#10943 = CARTESIAN_POINT ( 'NONE',  ( -2.500000000000000000, 3.500000000000000000, 0.6099999999999999867 ) ) ;
#10944 =( LENGTH_UNIT ( ) NAMED_UNIT ( * ) SI_UNIT ( .MILLI., .METRE. ) );
#10945 = ORIENTED_EDGE ( 'NONE', *, *, #7534, .F. ) ;
#10946 = VECTOR ( 'NONE', #10097, 1000.000000000000000 ) ;
#10947 = EDGE_LOOP ( 'NONE', ( #8238, #7429, #4392, #5705 ) ) ;
#10948 = VERTEX_POINT ( 'NONE', #11005 ) ;
#10949 = DIRECTION ( 'NONE',  ( 0.000000000000000000, 0.000000000000000000, -1.000000000000000000 ) ) ;
#10950 = CARTESIAN_POINT ( 'NONE',  ( 2.155845792290829621, -5.055296610169490279, 3.756158857535770057 ) ) ;
#10951 = ORIENTED_EDGE ( 'NONE', *, *, #5871, .T. ) ;
#10952 = CARTESIAN_POINT ( 'NONE',  ( 1.951437470830589938, -0.5429564742160228885, 3.384463041838829955 ) ) ;
#10953 = EDGE_CURVE ( 'NONE', #9321, #2413, #15686, .T. ) ;
#10954 = DIRECTION ( 'NONE',  ( 0.7045302523384989746, -0.08528919673497019349, -0.7045302523385029714 ) ) ;
#10955 = VECTOR ( 'NONE', #16902, 1000.000000000000000 ) ;
#10956 = CARTESIAN_POINT ( 'NONE',  ( -2.091095264232510242, -1.656953435693890198, 5.779845490516250628 ) ) ;
#10957 = ADVANCED_FACE ( 'NONE', ( #13700 ), #14995, .T. ) ;
#10958 = CARTESIAN_POINT ( 'NONE',  ( 0.6640878839024751956, -0.1379237288135599648, 7.269405042592523181 ) ) ;
#10959 = ORIENTED_EDGE ( 'NONE', *, *, #12979, .F. ) ;
#10960 = CARTESIAN_POINT ( 'NONE',  ( -1.943632316591239917, -0.5536016949152539057, 3.373048379518170048 ) ) ;
#10961 = EDGE_CURVE ( 'NONE', #412, #2630, #15185, .T. ) ;
#10962 = EDGE_CURVE ( 'NONE', #11846, #13146, #2493, .T. ) ;
#10963 = ORIENTED_EDGE ( 'NONE', *, *, #3475, .T. ) ;
#10964 = CARTESIAN_POINT ( 'NONE',  ( -2.519547246525518425, -0.2402542372881359412, 3.866491354109200529 ) ) ;
#10965 = ORIENTED_EDGE ( 'NONE', *, *, #5895, .F. ) ;
#10966 = CARTESIAN_POINT ( 'NONE',  ( -0.1749999999999999889, 9.500000000000000000, 3.100000000000000089 ) ) ;
#10967 = CARTESIAN_POINT ( 'NONE',  ( -2.075124426334558958, -2.918361879621430344, 5.810227140144560209 ) ) ;
#10968 = VECTOR ( 'NONE', #8505, 1000.000000000000000 ) ;
#10969 = CARTESIAN_POINT ( 'NONE',  ( 2.043308330018790198, -5.399788135593220240, 5.867646457774659652 ) ) ;
#10970 = CARTESIAN_POINT ( 'NONE',  ( 2.328527996529149657, -0.5662447625043111055, 3.426787111016343701 ) ) ;
#10971 = ORIENTED_EDGE ( 'NONE', *, *, #9043, .F. ) ;
#10972 = DIRECTION ( 'NONE',  ( 0.000000000000000000, 0.000000000000000000, 1.000000000000000000 ) ) ;
#10973 = CARTESIAN_POINT ( 'NONE',  ( -2.053221424930790295, -4.734848366107910600, 3.549770689668290125 ) ) ;
#10974 = CARTESIAN_POINT ( 'NONE',  ( -2.437122747866789840, -5.010466949207390108, 3.649501829874993941 ) ) ;
#10975 = LINE ( 'NONE', #16622, #11133 ) ;
#10976 = LINE ( 'NONE', #2539, #2143 ) ;
#10977 = PLANE ( 'NONE',  #9135 ) ;
#10978 = CARTESIAN_POINT ( 'NONE',  ( 0.6217226704572607066, -1.307629111369559949, 6.656620240022977697 ) ) ;
#10980 = EDGE_CURVE ( 'NONE', #2413, #8624, #8142, .T. ) ;
#10979 = DIRECTION ( 'NONE',  ( 1.306144734853129823E-16, -1.000000000000000000, 0.000000000000000000 ) ) ;
#10981 = ORIENTED_EDGE ( 'NONE', *, *, #15378, .F. ) ;
#10982 = LINE ( 'NONE', #16629, #8942 ) ;
#10983 = VECTOR ( 'NONE', #17786, 1000.000000000000000 ) ;
#10984 = CARTESIAN_POINT ( 'NONE',  ( -0.5999999999999999778, 7.347880794884128857E-17, 7.599999999999999645 ) ) ;
#10985 = CARTESIAN_POINT ( 'NONE',  ( 2.523518139275831462, -2.336154672414218592, 5.521565513971776085 ) ) ;
#10986 = CARTESIAN_POINT ( 'NONE',  ( -1.485788269501200132, -4.829629811528119099, 2.863981322975839738 ) ) ;
#10987 = CARTESIAN_POINT ( 'NONE',  ( 1.994315313497110997, -5.386440677966105817, 5.187224322759965922 ) ) ;
#10988 = ORIENTED_EDGE ( 'NONE', *, *, #878, .T. ) ;
#10989 = DIRECTION ( 'NONE',  ( -7.930164461608259947E-17, 0.000000000000000000, -1.000000000000000000 ) ) ;
#10990 = LINE ( 'NONE', #6824, #14432 ) ;
#10991 = CARTESIAN_POINT ( 'NONE',  ( 2.500000000000000000, 11.29999999999999893, 1.600000000000000089 ) ) ;
#10992 = ORIENTED_EDGE ( 'NONE', *, *, #5746, .F. ) ;
#10993 = CARTESIAN_POINT ( 'NONE',  ( 1.661700935788380074, -5.337500000000000355, 3.038299064211610112 ) ) ;
#10994 = CARTESIAN_POINT ( 'NONE',  ( 1.951437470830589938, -0.5429564742160228885, 3.384463041838829955 ) ) ;
#10995 = CARTESIAN_POINT ( 'NONE',  ( 1.769056124370469885, -3.915917399657852904, 2.721729512470748791 ) ) ;
#10996 = CARTESIAN_POINT ( 'NONE',  ( 2.616666666666660035, -5.805074450128190455E-17, 4.000000000000000000 ) ) ;
#10997 = CARTESIAN_POINT ( 'NONE',  ( -0.3509990757148119811, -1.125163681423229756, 6.722795464567655976 ) ) ;
#10999 = EDGE_CURVE ( 'NONE', #8884, #16183, #16654, .T. ) ;
#10998 = LINE ( 'NONE', #16647, #7010 ) ;
#11000 = DIRECTION ( 'NONE',  ( 1.000000000000000000, 0.000000000000000000, 0.000000000000000000 ) ) ;
#11001 = VERTEX_POINT ( 'NONE', #9326 ) ;
#11002 = LINE ( 'NONE', #18098, #14155 ) ;
#11003 = CARTESIAN_POINT ( 'NONE',  ( 1.407651048079441525, -0.3266949152542383272, 2.450250343405061759 ) ) ;
#11004 = CARTESIAN_POINT ( 'NONE',  ( 0.0003104168811309170268, -5.145080155286260393, 2.198280450787269746 ) ) ;
#11005 = CARTESIAN_POINT ( 'NONE',  ( 1.899999999999999911, 2.000000000000000000, 0.5999999999999999778 ) ) ;
#11006 = CARTESIAN_POINT ( 'NONE',  ( -1.128670402850159737, -5.470974576271190770, 7.101865548313641696 ) ) ;
#11007 = EDGE_LOOP ( 'NONE', ( #5423, #7700, #142, #1854 ) ) ;
#11008 = CYLINDRICAL_SURFACE ( 'NONE', #6046, 0.5000000000000004441 ) ;
#11009 = CARTESIAN_POINT ( 'NONE',  ( -1.851073041990159540, -5.193220338983048912, 6.153284478378270528 ) ) ;
#11010 = CARTESIAN_POINT ( 'NONE',  ( 1.750000000000000000, 0.5999999999999999778, 7.700000000000000178 ) ) ;
#11011 = LINE ( 'NONE', #8147, #5881 ) ;
#11012 = ORIENTED_EDGE ( 'NONE', *, *, #2125, .T. ) ;
#11013 = CARTESIAN_POINT ( 'NONE',  ( -1.092567884283820012, -4.637854336594780413, 6.784476218553590066 ) ) ;
#11014 = CARTESIAN_POINT ( 'NONE',  ( 0.6370285429020036139, -0.6606104644819236205, 2.105399314608770833 ) ) ;
#11015 = FACE_OUTER_BOUND ( 'NONE', #3305, .T. ) ;
#11016 = CARTESIAN_POINT ( 'NONE',  ( 2.500000000000000000, 2.000000000000000000, 1.600000000000000089 ) ) ;
#11017 = CARTESIAN_POINT ( 'NONE',  ( -1.000000000000000000, -5.000000000000000000, 6.100000000000000533 ) ) ;
#11018 = CARTESIAN_POINT ( 'NONE',  ( 2.211317922628870392, -2.472043525783979678, 3.894507149290419967 ) ) ;
#11019 = FACE_OUTER_BOUND ( 'NONE', #16304, .T. ) ;
#11020 = CARTESIAN_POINT ( 'NONE',  ( -1.673492459604430938, -3.496728210468663889, 3.510746103527421891 ) ) ;
#11021 = FACE_OUTER_BOUND ( 'NONE', #1219, .T. ) ;
#11022 = DIRECTION ( 'NONE',  ( -1.000000000000000000, 0.000000000000000000, 0.000000000000000000 ) ) ;
#11023 = ORIENTED_EDGE ( 'NONE', *, *, #7536, .T. ) ;
#11024 = VECTOR ( 'NONE', #9196, 1000.000000000000000 ) ;
#11025 = VECTOR ( 'NONE', #14994, 1000.000000000000000 ) ;
#11026 = CARTESIAN_POINT ( 'NONE',  ( 8.785293332290788772E-16, 10.80000000000000071, 7.700000000000000178 ) ) ;
#11027 = ORIENTED_EDGE ( 'NONE', *, *, #6636, .T. ) ;
#11028 = ORIENTED_EDGE ( 'NONE', *, *, #2132, .T. ) ;
#11029 = EDGE_LOOP ( 'NONE', ( #11680, #9441, #11890, #3876 ) ) ;
#11030 = LINE ( 'NONE', #8166, #12755 ) ;
#11031 = CARTESIAN_POINT ( 'NONE',  ( 0.7982439214406963357, -5.130932203389829915, 6.591424794228156081 ) ) ;
#11032 = CARTESIAN_POINT ( 'NONE',  ( 1.550000000000000044, -6.000000000000000000, 5.100000000000000533 ) ) ;
#11033 = FACE_OUTER_BOUND ( 'NONE', #5190, .T. ) ;
#11034 = DIRECTION ( 'NONE',  ( 6.123233995736769734E-17, 8.894960955186829541E-48, 1.000000000000000000 ) ) ;
#11035 = DIRECTION ( 'NONE',  ( 0.000000000000000000, 0.000000000000000000, 1.000000000000000000 ) ) ;
#11036 = PLANE ( 'NONE',  #3764 ) ;
#11037 = CARTESIAN_POINT ( 'NONE',  ( -2.036910256464079971, -4.940602084342534894, 4.443293066459140128 ) ) ;
#11038 = CARTESIAN_POINT ( 'NONE',  ( -0.07064654565474801085, -0.1512711864406789675, 7.352897294663512717 ) ) ;
#11039 = LINE ( 'NONE', #16688, #6132 ) ;
#11040 = ORIENTED_EDGE ( 'NONE', *, *, #16251, .T. ) ;
#11041 = CARTESIAN_POINT ( 'NONE',  ( -1.666450993087168930, -0.1824152542372889096, 6.765380371283871597 ) ) ;
#11042 = CARTESIAN_POINT ( 'NONE',  ( -1.250000000000000000, 3.881370849898470254, 5.100000000000000533 ) ) ;
#11043 = ORIENTED_EDGE ( 'NONE', *, *, #13307, .F. ) ;
#11044 = LINE ( 'NONE', #17874, #13249 ) ;
#11045 = CARTESIAN_POINT ( 'NONE',  ( 2.283153923255319739, -2.196424942684490400, 4.129076318403450685 ) ) ;
#11046 = CARTESIAN_POINT ( 'NONE',  ( 2.650076489488250697, -5.377542372881360500, 4.841243018609314497 ) ) ;
#11047 = EDGE_CURVE ( 'NONE', #4345, #12508, #1186, .T. ) ;
#11048 = CARTESIAN_POINT ( 'NONE',  ( -2.573461662271331551, -4.847448931189385135, 5.348389362822530302 ) ) ;
#11049 = VERTEX_POINT ( 'NONE', #7764 ) ;
#11050 = CARTESIAN_POINT ( 'NONE',  ( 0.03000000000000110217, 11.40000000000000036, 1.600000000000000089 ) ) ;
#11051 = EDGE_CURVE ( 'NONE', #7200, #2787, #13409, .T. ) ;
#11052 = CARTESIAN_POINT ( 'NONE',  ( 2.340959815966380031, -3.849893411152960354, 4.942183458383420103 ) ) ;
#11053 = CARTESIAN_POINT ( 'NONE',  ( -0.5355577887185811736, -4.567989471729919870, 7.299286738308172318 ) ) ;
#11054 = DIRECTION ( 'NONE',  ( 0.000000000000000000, 0.000000000000000000, -1.000000000000000000 ) ) ;
#11055 = LINE ( 'NONE', #12364, #14139 ) ;
#11056 = DIRECTION ( 'NONE',  ( 7.401486830834380223E-16, 1.000000000000000000, -1.110223024625159992E-16 ) ) ;
#11057 = CIRCLE ( 'NONE', #14312, 0.2000000000000000389 ) ;
#11058 = CARTESIAN_POINT ( 'NONE',  ( -1.727468145286550127, -1.633665147405598761, 5.809394271505101237 ) ) ;
#11059 = DIRECTION ( 'NONE',  ( 0.000000000000000000, 0.000000000000000000, -1.000000000000000000 ) ) ;
#11060 = ORIENTED_EDGE ( 'NONE', *, *, #13034, .F. ) ;
#11061 = CARTESIAN_POINT ( 'NONE',  ( 1.399999999999999911, -7.000000000000000000, 3.299999999999999822 ) ) ;
#11062 = PLANE ( 'NONE',  #17357 ) ;
#11063 = CARTESIAN_POINT ( 'NONE',  ( -0.9707742057416274273, -0.1735169491525429541, 6.508944043303927174 ) ) ;
#11064 = CARTESIAN_POINT ( 'NONE',  ( 1.650842931266089497, -2.033406924666469884, 2.622060802311419803 ) ) ;
#11065 = DIRECTION ( 'NONE',  ( 0.000000000000000000, -1.000000000000000000, -2.220446049250309876E-16 ) ) ;
#11066 = CARTESIAN_POINT ( 'NONE',  ( -0.2109711709854041328, -5.280843314568215874, 2.050669023674909663 ) ) ;
#11067 = CARTESIAN_POINT ( 'NONE',  ( -1.965557623688110933, -5.211016949152535993, 5.292675575926340414 ) ) ;
#11068 = VERTEX_POINT ( 'NONE', #2411 ) ;
#11069 = EDGE_CURVE ( 'NONE', #2860, #11926, #8058, .T. ) ;
#11070 = DIRECTION ( 'NONE',  ( 0.000000000000000000, -1.000000000000000000, 0.000000000000000000 ) ) ;
#11071 = AXIS2_PLACEMENT_3D ( 'NONE', #7494, #11847, #10441 ) ;
#11072 = LINE ( 'NONE', #14126, #8534 ) ;
#11073 = CARTESIAN_POINT ( 'NONE',  ( -1.149999999999999911, 9.299999999999998934, 7.500000000000000000 ) ) ;
#11074 = EDGE_CURVE ( 'NONE', #410, #11828, #6357, .T. ) ;
#11075 = VERTEX_POINT ( 'NONE', #13505 ) ;
#11076 = CARTESIAN_POINT ( 'NONE',  ( -2.011500846714319835, -5.551059322033900401, 3.478373409938470218 ) ) ;
#11077 = EDGE_CURVE ( 'NONE', #4535, #9612, #823, .T. ) ;
#11078 = CARTESIAN_POINT ( 'NONE',  ( -2.316126390218390618, -4.734848366107908824, 3.404364157709380390 ) ) ;
#11079 = CARTESIAN_POINT ( 'NONE',  ( 0.6890111762202997259, -3.799475958216412153, 2.137115435286760956 ) ) ;
#11080 = LINE ( 'NONE', #13953, #9395 ) ;
#11081 = CARTESIAN_POINT ( 'NONE',  ( 2.049150047780149642, -0.7059744922340407403, 4.826039376028505856 ) ) ;
#11082 = CARTESIAN_POINT ( 'NONE',  ( -1.899999999999999911, 9.199999999999999289, 0.5999999999999999778 ) ) ;
#11083 = ORIENTED_EDGE ( 'NONE', *, *, #17084, .F. ) ;
#11084 = LINE ( 'NONE', #16650, #12070 ) ;
#11085 = EDGE_CURVE ( 'NONE', #5300, #620, #12127, .T. ) ;
#11086 = CARTESIAN_POINT ( 'NONE',  ( -2.293398556041709835, -0.5358050847457630494, 4.171956209133480975 ) ) ;
#11087 = CARTESIAN_POINT ( 'NONE',  ( 2.340070819011249803, -0.3800847457627120063, 4.950151441910540129 ) ) ;
#11088 = CARTESIAN_POINT ( 'NONE',  ( 1.962536940652990003, -2.704926408666860294, 5.998920491814760503 ) ) ;
#11089 = DIRECTION ( 'NONE',  ( 0.000000000000000000, 0.000000000000000000, 1.000000000000000000 ) ) ;
#11090 = CARTESIAN_POINT ( 'NONE',  ( -1.800129581279449775, -5.564406779661021041, 2.750028594811118943 ) ) ;
#11091 = ORIENTED_EDGE ( 'NONE', *, *, #5177, .F. ) ;
#11092 = ORIENTED_EDGE ( 'NONE', *, *, #2728, .F. ) ;
#11093 = DIRECTION ( 'NONE',  ( -0.7071067811865475727, -2.050767998142408981E-32, -0.7071067811865475727 ) ) ;
#11094 = FACE_OUTER_BOUND ( 'NONE', #13173, .T. ) ;
#11095 = FACE_OUTER_BOUND ( 'NONE', #11509, .T. ) ;
#11096 = EDGE_CURVE ( 'NONE', #7698, #2828, #10334, .T. ) ;
#11097 = EDGE_LOOP ( 'NONE', ( #5325, #9936, #13077, #6278 ) ) ;
#11098 = CARTESIAN_POINT ( 'NONE',  ( 1.026235786675480099, -4.404971453711899798, 6.817920158464540137 ) ) ;
#11099 = CARTESIAN_POINT ( 'NONE',  ( 0.009452110982655418520, -5.000192044704539818, 2.350000000000000089 ) ) ;
#11100 = DIRECTION ( 'NONE',  ( 1.233581138472399909E-16, 6.167905692361979821E-17, -1.000000000000000000 ) ) ;
#11101 = FACE_OUTER_BOUND ( 'NONE', #13161, .T. ) ;
#11102 = CARTESIAN_POINT ( 'NONE',  ( -2.283153923255329953, -3.403575057315510133, 4.129076318403500423 ) ) ;
#11103 = CARTESIAN_POINT ( 'NONE',  ( -0.3750000000000000000, 6.450000000000000178, 2.100000000000000089 ) ) ;
#11104 = CARTESIAN_POINT ( 'NONE',  ( -2.035869680587120811, -3.310421904162345719, 4.964832940349540813 ) ) ;
#11105 = EDGE_CURVE ( 'NONE', #11415, #16121, #6924, .T. ) ;
#11106 = CARTESIAN_POINT ( 'NONE',  ( 1.899999999999999911, 4.700000000000000178, 0.5999999999999999778 ) ) ;
#11107 = DIRECTION ( 'NONE',  ( -2.220446049250309876E-16, 0.000000000000000000, -1.000000000000000000 ) ) ;
#11108 = ORIENTED_EDGE ( 'NONE', *, *, #15830, .F. ) ;
#11109 = ADVANCED_FACE ( 'NONE', ( #9703 ), #4229, .F. ) ;
#11110 = DIRECTION ( 'NONE',  ( 1.000000000000000000, 0.000000000000000000, 0.000000000000000000 ) ) ;
#11111 = VERTEX_POINT ( 'NONE', #9889 ) ;
#11112 = ORIENTED_EDGE ( 'NONE', *, *, #13683, .F. ) ;
#11113 = EDGE_CURVE ( 'NONE', #4627, #356, #78, .T. ) ;
#11114 = ORIENTED_EDGE ( 'NONE', *, *, #111, .F. ) ;
#11115 = LINE ( 'NONE', #4976, #7637 ) ;
#11116 = CARTESIAN_POINT ( 'NONE',  ( -1.754713504580578842, -5.251059322033895249, 3.634325740584633646 ) ) ;
#11117 = CARTESIAN_POINT ( 'NONE',  ( -0.4469859058769716786, -1.823812330071880705, 2.084026511420800976 ) ) ;
#11118 = AXIS2_PLACEMENT_3D ( 'NONE', #13991, #14076, #1506 ) ;
#11119 = FACE_OUTER_BOUND ( 'NONE', #1645, .T. ) ;
#11120 = CARTESIAN_POINT ( 'NONE',  ( 0.1749999999999999889, 6.799999999999999822, 1.600000000000000089 ) ) ;
#11121 = LINE ( 'NONE', #15679, #4597 ) ;
#11122 = PLANE ( 'NONE',  #9925 ) ;
#11123 = AXIS2_PLACEMENT_3D ( 'NONE', #2200, #12291, #5254 ) ;
#11124 = CARTESIAN_POINT ( 'NONE',  ( 0.5500000000000000444, 6.450000000000000178, 3.299999999999999822 ) ) ;
#11125 = CARTESIAN_POINT ( 'NONE',  ( 1.928817277882869829, -1.144611093351550091, 6.048484184565929844 ) ) ;
#11126 = CARTESIAN_POINT ( 'NONE',  ( -2.651721837666119796, -0.2269067796610169385, 4.594045830208265180 ) ) ;
#11127 = CARTESIAN_POINT ( 'NONE',  ( -1.811729841638700211, -0.5580508474576270084, 3.197954009834299782 ) ) ;
#11128 = ORIENTED_EDGE ( 'NONE', *, *, #8577, .T. ) ;
#11129 = CARTESIAN_POINT ( 'NONE',  ( 1.647941990407678636, -0.04449152542372906277, 3.475676388127089123 ) ) ;
#11130 = CARTESIAN_POINT ( 'NONE',  ( 0.3042893218813439438, 6.450000000000000178, 2.029289321881350361 ) ) ;
#11131 = ORIENTED_EDGE ( 'NONE', *, *, #9352, .T. ) ;
#11132 = CYLINDRICAL_SURFACE ( 'NONE', #9095, 1.016666666666670160 ) ;
#11133 = VECTOR ( 'NONE', #12453, 1000.000000000000000 ) ;
#11134 = CARTESIAN_POINT ( 'NONE',  ( -1.353103843060629918, -2.801920438179980266, 6.625579309552958485 ) ) ;
#11135 = DIRECTION ( 'NONE',  ( 0.000000000000000000, 0.000000000000000000, 1.000000000000000000 ) ) ;
#11136 = CARTESIAN_POINT ( 'NONE',  ( -2.458531667407850563, -5.506567796610171150, 5.699238225248945966 ) ) ;
#11137 = ORIENTED_EDGE ( 'NONE', *, *, #13145, .T. ) ;
#11138 = CARTESIAN_POINT ( 'NONE',  ( 0.2818998297622880012, -1.354205687946139935, 7.036509827384409554 ) ) ;
#11139 = AXIS2_PLACEMENT_3D ( 'NONE', #13812, #952, #9556 ) ;
#11140 = CARTESIAN_POINT ( 'NONE',  ( -2.034805890357269220, -0.5313559322033900578, 4.427518626519226785 ) ) ;
#11141 = VECTOR ( 'NONE', #1548, 1000.000000000000000 ) ;
#11142 = ADVANCED_FACE ( 'NONE', ( #15548 ), #5613, .T. ) ;
#11143 = ORIENTED_EDGE ( 'NONE', *, *, #5942, .F. ) ;
#11144 = CARTESIAN_POINT ( 'NONE',  ( 4.898587196589409994E-17, 0.1000000000000000056, 8.300000000000000711 ) ) ;
#11145 = DIRECTION ( 'NONE',  ( 2.261565420532729920E-16, 1.000000000000000000, 0.000000000000000000 ) ) ;
#11146 = CARTESIAN_POINT ( 'NONE',  ( -1.491388273268980491, -1.587088570829020551, 6.110908523251552538 ) ) ;
#11147 = EDGE_CURVE ( 'NONE', #13226, #16249, #13013, .T. ) ;
#11148 = DIRECTION ( 'NONE',  ( 6.049014748177260544E-16, -2.493473113004680074E-16, 1.000000000000000000 ) ) ;
#11149 = VECTOR ( 'NONE', #3865, 1000.000000000000000 ) ;
#11150 = ORIENTED_EDGE ( 'NONE', *, *, #18289, .T. ) ;
#11151 = DIRECTION ( 'NONE',  ( -0.7071067811865470176, -9.235837992257497283E-17, 0.7071067811865480168 ) ) ;
#11152 = VECTOR ( 'NONE', #1595, 1000.000000000000000 ) ;
#11153 = DIRECTION ( 'NONE',  ( 5.551115123125790591E-16, -9.251858538542978977E-17, 1.000000000000000000 ) ) ;
#11154 = AXIS2_PLACEMENT_3D ( 'NONE', #288, #10173, #15837 ) ;
#11155 = CARTESIAN_POINT ( 'NONE',  ( 1.392767620582681332, -3.570433951693503527, 2.440948861123688474 ) ) ;
#11156 = EDGE_CURVE ( 'NONE', #8261, #9511, #15398, .T. ) ;
#11157 = VECTOR ( 'NONE', #6959, 1000.000000000000000 ) ;
#11158 = PRESENTATION_LAYER_ASSIGNMENT (  '', '', ( #16775 ) ) ;
#11159 = CARTESIAN_POINT ( 'NONE',  ( -0.009452110982656853136, -5.299807955295470663, 2.649999999999998579 ) ) ;
#11160 = CARTESIAN_POINT ( 'NONE',  ( 1.679950111053631900, -5.404237288135596451, 5.880020650119711867 ) ) ;
#11161 = ORIENTED_EDGE ( 'NONE', *, *, #10545, .T. ) ;
#11162 = VECTOR ( 'NONE', #8549, 1000.000000000000000 ) ;
#11163 = FACE_OUTER_BOUND ( 'NONE', #3673, .T. ) ;
#11164 = CARTESIAN_POINT ( 'NONE',  ( 1.899999999999999911, 2.799999999999999822, 0.6099999999999999867 ) ) ;
#11165 = CARTESIAN_POINT ( 'NONE',  ( -1.496290472746829803, -0.5672554343907050267, 2.872674968141029961 ) ) ;
#11166 = ORIENTED_EDGE ( 'NONE', *, *, #2594, .T. ) ;
#11167 = VECTOR ( 'NONE', #2925, 1000.000000000000000 ) ;
#11168 = CARTESIAN_POINT ( 'NONE',  ( 0.5999999999999999778, -1.110223024625159992E-16, 7.599999999999999645 ) ) ;
#11169 = CARTESIAN_POINT ( 'NONE',  ( 2.296954468777709923, -0.6361096273691760894, 4.187412587068650716 ) ) ;
#11170 = DIRECTION ( 'NONE',  ( -0.2800000000000001377, 0.9599999999999999645, 0.000000000000000000 ) ) ;
#11171 = CARTESIAN_POINT ( 'NONE',  ( 1.861802609626429961, -0.7991276453871953844, 5.565212624397201324 ) ) ;
#11172 = AXIS2_PLACEMENT_3D ( 'NONE', #7752, #16451, #13397 ) ;
#11173 = CIRCLE ( 'NONE', #5566, 0.2000000000000005107 ) ;
#11174 = CARTESIAN_POINT ( 'NONE',  ( 1.000000000000000000, 6.799999999999999822, 7.700000000000000178 ) ) ;
#11175 = EDGE_CURVE ( 'NONE', #17218, #3339, #2852, .T. ) ;
#11176 = EDGE_LOOP ( 'NONE', ( #15864, #8820, #2698, #2769 ) ) ;
#11177 = PRODUCT_RELATED_PRODUCT_CATEGORY ( 'part', '', ( #9637 ) ) ;
#11178 = EDGE_CURVE ( 'NONE', #6296, #458, #1470, .T. ) ;
#11179 = AXIS2_PLACEMENT_3D ( 'NONE', #6909, #8482, #1453 ) ;
#11180 = CARTESIAN_POINT ( 'NONE',  ( 1.661700935788380074, -5.337500000000000355, 3.038299064211610112 ) ) ;
#11181 = AXIS2_PLACEMENT_3D ( 'NONE', #14079, #114, #8631 ) ;
#11182 = CARTESIAN_POINT ( 'NONE',  ( -2.350067830300900162, -0.5224576271186440746, 4.825253242917699303 ) ) ;
#11183 = EDGE_CURVE ( 'NONE', #17929, #3526, #2955, .T. ) ;
#11184 = CARTESIAN_POINT ( 'NONE',  ( -1.332058588847369940, -3.100827309567760537, 6.640197310420220767 ) ) ;
#11185 = DIRECTION ( 'NONE',  ( 1.445602896647339508E-15, 1.000000000000000000, 1.332267629550190412E-15 ) ) ;
#11186 = ADVANCED_FACE ( 'NONE', ( #4141 ), #15459, .T. ) ;
#11187 = DIRECTION ( 'NONE',  ( -4.906538933386810061E-16, -1.000000000000000000, 0.000000000000000000 ) ) ;
#11188 = ORIENTED_EDGE ( 'NONE', *, *, #10243, .T. ) ;
#11189 = ORIENTED_EDGE ( 'NONE', *, *, #17749, .F. ) ;
#11190 = CARTESIAN_POINT ( 'NONE',  ( -1.428515267734879579, -5.268855932203389436, 2.829745655876930499 ) ) ;
#11191 = CARTESIAN_POINT ( 'NONE',  ( 0.000000000000000000, 0.000000000000000000, 0.000000000000000000 ) ) ;
#11192 = VECTOR ( 'NONE', #10331, 1000.000000000000000 ) ;
#11193 = DIRECTION ( 'NONE',  ( 1.110223024625159992E-16, 0.000000000000000000, -1.000000000000000000 ) ) ;
#11194 = VECTOR ( 'NONE', #16025, 1000.000000000000000 ) ;
#11195 = ORIENTED_EDGE ( 'NONE', *, *, #9930, .F. ) ;
#11196 = CARTESIAN_POINT ( 'NONE',  ( 0.1824815401350060040, -4.498124606865050445, 7.046368721022729709 ) ) ;
#11197 = CIRCLE ( 'NONE', #14446, 0.2500000000000002220 ) ;
#11198 = CARTESIAN_POINT ( 'NONE',  ( -0.7999999999998730349, 12.00000000000000000, -9.797174393178840942E-17 ) ) ;
#11199 = CARTESIAN_POINT ( 'NONE',  ( -0.009452110982655139229, -5.299807955295460005, 2.350000000000000089 ) ) ;
#11200 = CARTESIAN_POINT ( 'NONE',  ( 1.000000000000000000, -5.000000000000000000, 3.299999999999999822 ) ) ;
#11201 = PLANE ( 'NONE',  #13519 ) ;
#11202 = CARTESIAN_POINT ( 'NONE',  ( -1.777964140657649850, -4.731007489747940831, 6.241943319976260618 ) ) ;
#11203 = AXIS2_PLACEMENT_3D ( 'NONE', #357, #3221, #3310 ) ;
#11204 = FACE_OUTER_BOUND ( 'NONE', #1253, .T. ) ;
#11205 = VECTOR ( 'NONE', #8805, 1000.000000000000000 ) ;
#11206 = CARTESIAN_POINT ( 'NONE',  ( -0.2302241296435190154, -3.706322805063249959, 2.659926792304259990 ) ) ;
#11207 = EDGE_CURVE ( 'NONE', #13279, #12720, #2767, .T. ) ;
#11208 = FACE_BOUND ( 'NONE', #7082, .T. ) ;
#11209 = ORIENTED_EDGE ( 'NONE', *, *, #3364, .T. ) ;
#11210 = CYLINDRICAL_SURFACE ( 'NONE', #879, 0.01000000000000002623 ) ;
#11211 = ORIENTED_EDGE ( 'NONE', *, *, #8370, .T. ) ;
#11212 = AXIS2_PLACEMENT_3D ( 'NONE', #15965, #14556, #17053 ) ;
#11213 =( NAMED_UNIT ( * ) PLANE_ANGLE_UNIT ( ) SI_UNIT ( $, .RADIAN. ) );
#11214 = VERTEX_POINT ( 'NONE', #7024 ) ;
#11215 = ORIENTED_EDGE ( 'NONE', *, *, #17956, .F. ) ;
#11216 = ORIENTED_EDGE ( 'NONE', *, *, #4273, .F. ) ;
#11217 = CARTESIAN_POINT ( 'NONE',  ( 1.800000000000000044, 12.00000000000000000, 1.600000000000000089 ) ) ;
#11218 = VECTOR ( 'NONE', #3516, 1000.000000000000000 ) ;
#11219 = CARTESIAN_POINT ( 'NONE',  ( -1.088937603231280304, -5.273305084745764759, 2.959627624143549074 ) ) ;
#11220 = CARTESIAN_POINT ( 'NONE',  ( -1.889999999999999902, 3.500000000000000000, 0.6099999999999999867 ) ) ;
#11221 = DIRECTION ( 'NONE',  ( 1.110223024625159992E-16, 0.000000000000000000, -1.000000000000000000 ) ) ;
#11222 = CARTESIAN_POINT ( 'NONE',  ( -0.1749999999999999889, 8.200000000000001066, -3.200000000000000178 ) ) ;
#11223 = DIRECTION ( 'NONE',  ( 1.224646799147350002E-16, 1.000000000000000000, 0.000000000000000000 ) ) ;
#11224 = AXIS2_PLACEMENT_3D ( 'NONE', #1064, #11056, #5332 ) ;
#11225 = CARTESIAN_POINT ( 'NONE',  ( 1.800000000000000044, 8.881784197001260212E-17, 9.441371669411539713 ) ) ;
#11226 = CARTESIAN_POINT ( 'NONE',  ( 1.687170344132030042, -2.751502985243429844, 6.340793075730549511 ) ) ;
#11227 = CARTESIAN_POINT ( 'NONE',  ( 1.313542260532459149, -2.475884402143949892, 6.277817661335856059 ) ) ;
#11228 = CARTESIAN_POINT ( 'NONE',  ( -1.713314936023349944, -0.2610169491525429764, 3.089913064446579760 ) ) ;
#11229 = EDGE_CURVE ( 'NONE', #3622, #3076, #8412, .T. ) ;
#11230 = ORIENTED_EDGE ( 'NONE', *, *, #13426, .F. ) ;
#11231 = CARTESIAN_POINT ( 'NONE',  ( -2.500000000000000000, 0.4000000000000000222, 7.649999999999999467 ) ) ;
#11232 = AXIS2_PLACEMENT_3D ( 'NONE', #1662, #12959, #8787 ) ;
#11233 = DIRECTION ( 'NONE',  ( 6.123233995736764803E-17, -1.000000000000000000, 0.000000000000000000 ) ) ;
#11234 = ORIENTED_EDGE ( 'NONE', *, *, #12436, .T. ) ;
#11235 = CARTESIAN_POINT ( 'NONE',  ( -1.477796163681079911, -0.1824152542372889929, 6.531563725478150673 ) ) ;
#11236 = CARTESIAN_POINT ( 'NONE',  ( -0.1569242594330230167, -1.400782264522720144, 7.048216443236290374 ) ) ;
#11237 = ORIENTED_EDGE ( 'NONE', *, *, #11988, .F. ) ;
#11238 = DIRECTION ( 'NONE',  ( 0.000000000000000000, -1.000000000000000000, 0.000000000000000000 ) ) ;
#11239 = VERTEX_POINT ( 'NONE', #1191 ) ;
#11240 = CARTESIAN_POINT ( 'NONE',  ( -0.3413183941262150078, -2.685478996738541291, 7.028571974690709823 ) ) ;
#11241 =( NAMED_UNIT ( * ) SI_UNIT ( $, .STERADIAN. ) SOLID_ANGLE_UNIT ( ) );
#11242 = CARTESIAN_POINT ( 'NONE',  ( 2.304156201936080617, -5.399788135593215799, 6.016707707703351282 ) ) ;
#11243 = ORIENTED_EDGE ( 'NONE', *, *, #10008, .T. ) ;
#11244 = CARTESIAN_POINT ( 'NONE',  ( 0.9170541073686970801, -1.284340823081270067, 6.867431071947180499 ) ) ;
#11245 = VECTOR ( 'NONE', #16464, 1000.000000000000000 ) ;
#11246 = CARTESIAN_POINT ( 'NONE',  ( 1.614765845140360589, -0.4067796610169500116, 5.967758800287426446 ) ) ;
#11247 = ORIENTED_EDGE ( 'NONE', *, *, #4824, .T. ) ;
#11248 = DIRECTION ( 'NONE',  ( -7.930164461608259947E-17, 0.000000000000000000, -1.000000000000000000 ) ) ;
#11249 = DIRECTION ( 'NONE',  ( 1.224646799147350002E-16, -1.000000000000000000, -6.123233995736769734E-17 ) ) ;
#11250 = DIRECTION ( 'NONE',  ( 1.000000000000000000, 8.615382147616920419E-16, 0.000000000000000000 ) ) ;
#11251 = CARTESIAN_POINT ( 'NONE',  ( -0.5133516189064535329, -1.447358841099289251, 6.687805814961367723 ) ) ;
#11252 = CARTESIAN_POINT ( 'NONE',  ( 1.550000000000000044, -5.599999999999999645, 6.100000000000000533 ) ) ;
#11253 = EDGE_LOOP ( 'NONE', ( #17495, #5271, #18288, #16411 ) ) ;
#11254 = CARTESIAN_POINT ( 'NONE',  ( 1.000000000000000000, -5.599999999999999645, 3.673738709727309981 ) ) ;
#11255 = FACE_OUTER_BOUND ( 'NONE', #6944, .T. ) ;
#11256 = CARTESIAN_POINT ( 'NONE',  ( 0.3803919826356921829, -0.3088983050847459166, 2.682580100125298461 ) ) ;
#11257 = CARTESIAN_POINT ( 'NONE',  ( 1.963178672446078687, -3.640298816558361406, 2.914210764660420061 ) ) ;
#11258 = ORIENTED_EDGE ( 'NONE', *, *, #12223, .T. ) ;
#11259 = AXIS2_PLACEMENT_3D ( 'NONE', #8861, #13121, #1991 ) ;
#11260 = CARTESIAN_POINT ( 'NONE',  ( -0.1654173910288039839, -5.280843314568230085, 2.650679959339568459 ) ) ;
#11261 = CARTESIAN_POINT ( 'NONE',  ( -1.489797906646480596, -5.188771186440680694, 6.112509577910826941 ) ) ;
#11262 = ORIENTED_EDGE ( 'NONE', *, *, #6642, .T. ) ;
#11263 = CARTESIAN_POINT ( 'NONE',  ( 1.500000000000000000, -5.599999999999999645, 2.299999999999999822 ) ) ;
#11264 = CARTESIAN_POINT ( 'NONE',  ( 2.234315482767910144, -5.359745762711869865, 3.960850823455320580 ) ) ;
#11265 = CARTESIAN_POINT ( 'NONE',  ( -0.009452110982655708218, -0.5998079552954630467, 2.350000000000000089 ) ) ;
#11266 = ORIENTED_EDGE ( 'NONE', *, *, #7770, .T. ) ;
#11267 = CARTESIAN_POINT ( 'NONE',  ( 0.7500000000000000000, 6.450000000000000178, 2.699264068711930253 ) ) ;
#11268 = CARTESIAN_POINT ( 'NONE',  ( 0.2620510901103109691, -1.893677194936739916, 2.361180871966390260 ) ) ;
#11269 = CARTESIAN_POINT ( 'NONE',  ( 0.5291502622129179434, 0.1000000000000000056, 7.700000000000000178 ) ) ;
#11270 = AXIS2_PLACEMENT_3D ( 'NONE', #3117, #15908, #16006 ) ;
#11271 = CARTESIAN_POINT ( 'NONE',  ( -1.508881462028629716, -1.288181699441250050, 6.092184821126286565 ) ) ;
#11272 = LINE ( 'NONE', #6833, #7587 ) ;
#11273 = VERTEX_POINT ( 'NONE', #5449 ) ;
#11274 = DIRECTION ( 'NONE',  ( -0.9396926207859082059, 3.797186380057531567E-16, -0.3420201433256691015 ) ) ;
#11275 = CARTESIAN_POINT ( 'NONE',  ( -2.155845792290839835, -0.5447033898305089217, 3.756158857535780271 ) ) ;
#11276 = CARTESIAN_POINT ( 'NONE',  ( -1.791574935211209807, -0.4913135593220339659, 6.226029630577610163 ) ) ;
#11277 = CARTESIAN_POINT ( 'NONE',  ( -2.326448859701059746, -3.380286769027220029, 4.344498395672320434 ) ) ;
#11278 = CARTESIAN_POINT ( 'NONE',  ( 6.858022075225179538E-16, -5.000000000000000000, -3.061616997868380183E-16 ) ) ;
#11279 = DIRECTION ( 'NONE',  ( -3.861645303044020177E-16, -1.000000000000000000, 1.268826313857319964E-16 ) ) ;
#11280 = CARTESIAN_POINT ( 'NONE',  ( -2.540842781840720654, -5.511016949152534927, 5.466141598148674952 ) ) ;
#11281 = ORIENTED_EDGE ( 'NONE', *, *, #15760, .T. ) ;
#11282 = ORIENTED_EDGE ( 'NONE', *, *, #11085, .F. ) ;
#11283 = CARTESIAN_POINT ( 'NONE',  ( -0.8570167067220348933, -5.282203389830509188, 2.508190348879360432 ) ) ;
#11284 = LINE ( 'NONE', #17008, #2638 ) ;
#11285 = DIRECTION ( 'NONE',  ( 0.000000000000000000, 0.000000000000000000, -1.000000000000000000 ) ) ;
#11286 = ORIENTED_EDGE ( 'NONE', *, *, #2249, .T. ) ;
#11287 = CARTESIAN_POINT ( 'NONE',  ( -0.9038768003981948462, -1.470647129387581575, 7.195219513931347954 ) ) ;
#11288 = EDGE_CURVE ( 'NONE', #17654, #4420, #11838, .T. ) ;
#11289 = CARTESIAN_POINT ( 'NONE',  ( 0.9724415447670879953, -0.7068739681193980662, 2.553509270169310064 ) ) ;
#11290 = CARTESIAN_POINT ( 'NONE',  ( 1.661700935788380074, -5.337500000000000355, 3.038299064211610112 ) ) ;
#11291 = EDGE_CURVE ( 'NONE', #8865, #16897, #5636, .T. ) ;
#11292 = CARTESIAN_POINT ( 'NONE',  ( -0.5500000000000000444, 3.050000000000000266, 2.699264068711930253 ) ) ;
#11293 = CARTESIAN_POINT ( 'NONE',  ( 2.239137794397009884, -0.6128213390808879835, 3.975425900939169921 ) ) ;
#11294 = EDGE_CURVE ( 'NONE', #2415, #6533, #12847, .T. ) ;
#11295 = DIRECTION ( 'NONE',  ( -0.7071067811865480168, 0.000000000000000000, -0.7071067811865470176 ) ) ;
#11296 = CARTESIAN_POINT ( 'NONE',  ( 0.4005155088302400634, -4.474836318576759453, 7.019123328904770531 ) ) ;
#11297 = ADVANCED_BREP_SHAPE_REPRESENTATION ( '', ( #8348, #17681 ), #4692 ) ;
#11298 = CARTESIAN_POINT ( 'NONE',  ( -1.124021676335500208, -3.589881363621813648, 2.982013645643241340 ) ) ;
#11299 = CARTESIAN_POINT ( 'NONE',  ( 1.889999999999999902, 4.700000000000000178, 0.6099999999999999867 ) ) ;
#11300 = ORIENTED_EDGE ( 'NONE', *, *, #8590, .T. ) ;
#11301 = CARTESIAN_POINT ( 'NONE',  ( -1.305383194095490307, -0.5672554343907051377, 3.106059597508353143 ) ) ;
#11302 = EDGE_LOOP ( 'NONE', ( #4462, #750, #14246, #16023 ) ) ;
#11303 = DIRECTION ( 'NONE',  ( 1.224646799147350002E-16, -1.000000000000000000, -6.123233995736769734E-17 ) ) ;
#11304 = SURFACE_STYLE_FILL_AREA ( #17024 ) ;
#11305 = ORIENTED_EDGE ( 'NONE', *, *, #10619, .T. ) ;
#11306 = LINE ( 'NONE', #12792, #13554 ) ;
#11307 = VECTOR ( 'NONE', #13582, 1000.000000000000000 ) ;
#11308 = EDGE_CURVE ( 'NONE', #11068, #17532, #16920, .T. ) ;
#11309 = ORIENTED_EDGE ( 'NONE', *, *, #15257, .F. ) ;
#11310 = CARTESIAN_POINT ( 'NONE',  ( 1.134881315981519645, -5.122033898305085486, 6.410767520434657918 ) ) ;
#11311 = CARTESIAN_POINT ( 'NONE',  ( 2.295344368707611160, -2.126560077819629413, 3.367893426919545519 ) ) ;
#11312 = EDGE_CURVE ( 'NONE', #10145, #17164, #7691, .T. ) ;
#11313 = CARTESIAN_POINT ( 'NONE',  ( -4.898587196589400133E-17, 6.700000000000000178, 6.599999999999999645 ) ) ;
#11314 = CARTESIAN_POINT ( 'NONE',  ( 1.763960074743270212, -0.6810390010611521161, 2.931777988865699847 ) ) ;
#11315 = EDGE_CURVE ( 'NONE', #4745, #15319, #3377, .T. ) ;
#11316 = DIRECTION ( 'NONE',  ( 6.167905692361979821E-17, 0.000000000000000000, 1.000000000000000000 ) ) ;
#11317 = DIRECTION ( 'NONE',  ( -1.000000000000000000, -1.331202777560457422E-30, -0.000000000000000000 ) ) ;
#11318 = LINE ( 'NONE', #7162, #11757 ) ;
#11319 = DIRECTION ( 'NONE',  ( -1.000000000000000000, 0.000000000000000000, 0.000000000000000000 ) ) ;
#11320 = CARTESIAN_POINT ( 'NONE',  ( -1.417709711196470046, -2.006277760018209566, 2.821478011237799954 ) ) ;
#11321 = CARTESIAN_POINT ( 'NONE',  ( 1.160665242129880426, -2.499172690432241772, 6.393445611272976947 ) ) ;
#11322 = CARTESIAN_POINT ( 'NONE',  ( -2.286166334984490067, -0.2135593220338989906, 5.258525443163870605 ) ) ;
#11323 = AXIS2_PLACEMENT_3D ( 'NONE', #4206, #16802, #2829 ) ;
#11324 = CARTESIAN_POINT ( 'NONE',  ( -1.149999999999999911, 9.248236190979499227, 7.693185165257809821 ) ) ;
#11325 = FACE_OUTER_BOUND ( 'NONE', #10342, .T. ) ;
#11326 = ORIENTED_EDGE ( 'NONE', *, *, #14183, .F. ) ;
#11327 = CARTESIAN_POINT ( 'NONE',  ( 1.622657008870240762E-16, -3.053113317719175556E-16, 2.649999999999998579 ) ) ;
#11328 = CARTESIAN_POINT ( 'NONE',  ( 0.4539185741479240255, -2.215872354612800521, 2.390735265170440105 ) ) ;
#11329 = ORIENTED_EDGE ( 'NONE', *, *, #15495, .T. ) ;
#11330 = CARTESIAN_POINT ( 'NONE',  ( 2.500000000000000000, 10.00000000000000000, 1.600000000000000089 ) ) ;
#11331 = ORIENTED_EDGE ( 'NONE', *, *, #13042, .T. ) ;
#11332 = EDGE_CURVE ( 'NONE', #6891, #12909, #4720, .T. ) ;
#11333 = CARTESIAN_POINT ( 'NONE',  ( -2.100188519621618788, -1.590929447189000090, 3.637948273607420457 ) ) ;
#11334 = CARTESIAN_POINT ( 'NONE',  ( 2.431060148753489081, -5.355296610169490101, 3.635668498923322112 ) ) ;
#11335 = EDGE_CURVE ( 'NONE', #1432, #2090, #13027, .T. ) ;
#11336 = ORIENTED_EDGE ( 'NONE', *, *, #17684, .F. ) ;
#11337 = CARTESIAN_POINT ( 'NONE',  ( 2.331386066015260106, -0.9583047870452390260, 4.378465089518139841 ) ) ;
#11338 = CARTESIAN_POINT ( 'NONE',  ( 1.965557623688110933, -0.3889830508474575455, 5.292675575926325315 ) ) ;
#11339 = ORIENTED_EDGE ( 'NONE', *, *, #1913, .F. ) ;
#11340 = LINE ( 'NONE', #5959, #10836 ) ;
#11341 = DIRECTION ( 'NONE',  ( 1.000000000000000000, -1.850371707708589879E-16, 0.000000000000000000 ) ) ;
#11342 = CARTESIAN_POINT ( 'NONE',  ( -1.899999999999999911, 4.700000000000000178, 0.5999999999999999778 ) ) ;
#11343 = CARTESIAN_POINT ( 'NONE',  ( 0.9361665894546294941, -2.285737219477670390, 2.872845392579769452 ) ) ;
#11344 = DIRECTION ( 'NONE',  ( 0.000000000000000000, 0.000000000000000000, -1.000000000000000000 ) ) ;
#11345 = CARTESIAN_POINT ( 'NONE',  ( 2.386628511786341722, -0.3533898305084745561, 3.539457309197775459 ) ) ;
#11346 = ORIENTED_EDGE ( 'NONE', *, *, #11312, .F. ) ;
#11347 = DIRECTION ( 'NONE',  ( 0.7049180327868849183, -0.7092887755011130224, 0.000000000000000000 ) ) ;
#11348 = LINE ( 'NONE', #4207, #17953 ) ;
#11349 = VECTOR ( 'NONE', #432, 1000.000000000000000 ) ;
#11350 = ORIENTED_EDGE ( 'NONE', *, *, #17159, .F. ) ;
#11351 = CARTESIAN_POINT ( 'NONE',  ( 0.009452110982653675123, -5.000192044704546035, 2.050000000000001155 ) ) ;
#11352 = CARTESIAN_POINT ( 'NONE',  ( 2.351526912647309953, -5.373093220338979847, 4.606040641882800379 ) ) ;
#11353 = ORIENTED_EDGE ( 'NONE', *, *, #7413, .T. ) ;
#11354 = DIRECTION ( 'NONE',  ( 1.000000000000000000, 0.000000000000000000, -2.220446049250319983E-16 ) ) ;
#11355 = CARTESIAN_POINT ( 'NONE',  ( 1.112838723655040107, -5.426483050847459744, 6.773667561836210105 ) ) ;
#11356 = LINE ( 'NONE', #9785, #2570 ) ;
#11357 = EDGE_CURVE ( 'NONE', #13417, #15242, #3253, .T. ) ;
#11358 = ORIENTED_EDGE ( 'NONE', *, *, #12878, .T. ) ;
#11359 = CARTESIAN_POINT ( 'NONE',  ( 2.500000000000000000, 4.700000000000000178, 1.600000000000000089 ) ) ;
#11360 = CARTESIAN_POINT ( 'NONE',  ( 1.630481553867769939, -2.056695212954759988, 3.002862530617850023 ) ) ;
#11361 = DIRECTION ( 'NONE',  ( 1.224646799147350002E-16, -1.000000000000000000, -6.123233995736779594E-17 ) ) ;
#11362 = CARTESIAN_POINT ( 'NONE',  ( 0.7854158957161911925, -1.963542059801608897, 2.803154272645130618 ) ) ;
#11363 = PLANE ( 'NONE',  #9055 ) ;
#11364 = VERTEX_POINT ( 'NONE', #9021 ) ;
#11365 = PLANE ( 'NONE',  #8250 ) ;
#11366 = CARTESIAN_POINT ( 'NONE',  ( 2.645377369053839356, -0.07118644067796667252, 4.488260618344900088 ) ) ;
#11367 = CARTESIAN_POINT ( 'NONE',  ( 1.167621112247380077, -2.821367850108300157, 6.743381174846749815 ) ) ;
#11368 = CARTESIAN_POINT ( 'NONE',  ( 1.750000000000000000, 11.40000000000000036, 7.550000000000000711 ) ) ;
#11369 = DIRECTION ( 'NONE',  ( -6.123233995736794386E-17, 0.000000000000000000, -1.000000000000000000 ) ) ;
#11370 = CARTESIAN_POINT ( 'NONE',  ( -0.4917262214559124933, -5.291101694915254505, 2.092115739186370948 ) ) ;
#11371 = ORIENTED_EDGE ( 'NONE', *, *, #13224, .T. ) ;
#11372 = ORIENTED_EDGE ( 'NONE', *, *, #7576, .F. ) ;
#11373 = CARTESIAN_POINT ( 'NONE',  ( 1.899999999999999911, 0.7500000000000000000, 7.649999999999999467 ) ) ;
#11374 = LINE ( 'NONE', #6492, #2934 ) ;
#11375 = LINE ( 'NONE', #17097, #16207 ) ;
#11376 = VERTEX_POINT ( 'NONE', #14672 ) ;
#11377 = LINE ( 'NONE', #1376, #7028 ) ;
#11378 = PRESENTATION_LAYER_ASSIGNMENT (  '', '', ( #1035 ) ) ;
#11379 = DIRECTION ( 'NONE',  ( -1.000000000000000000, 0.000000000000000000, 0.000000000000000000 ) ) ;
#11380 = CARTESIAN_POINT ( 'NONE',  ( -1.864786684738369837, -4.804713230972779137, 2.817120744449669978 ) ) ;
#11381 = ADVANCED_FACE ( 'NONE', ( #12936 ), #1740, .F. ) ;
#11382 = LINE ( 'NONE', #1378, #11729 ) ;
#11383 = CARTESIAN_POINT ( 'NONE',  ( -1.282210379528740063, -4.661142624883069630, 6.673494927815290190 ) ) ;
#11384 = CARTESIAN_POINT ( 'NONE',  ( 1.836970198721020197E-17, 3.581751045813930112, 7.700000000000000178 ) ) ;
#11385 = CARTESIAN_POINT ( 'NONE',  ( 1.217499609005879613, -3.892629111369556139, 3.046943272389411206 ) ) ;
#11386 = DIRECTION ( 'NONE',  ( -2.537652627714639929E-16, -1.000000000000000000, 0.000000000000000000 ) ) ;
#11387 = ORIENTED_EDGE ( 'NONE', *, *, #11357, .F. ) ;
#11388 = DIRECTION ( 'NONE',  ( 1.480297366166879989E-16, -1.000000000000000000, -1.480297366166879989E-16 ) ) ;
#11389 = ORIENTED_EDGE ( 'NONE', *, *, #15608, .T. ) ;
#11390 = EDGE_CURVE ( 'NONE', #7550, #11068, #11544, .T. ) ;
#11391 = EDGE_LOOP ( 'NONE', ( #16495, #2726, #2535, #3026 ) ) ;
#11392 = ADVANCED_FACE ( 'NONE', ( #17260 ), #4575, .T. ) ;
#11393 = FACE_OUTER_BOUND ( 'NONE', #4898, .T. ) ;
#11394 = CARTESIAN_POINT ( 'NONE',  ( -0.5291502622129179434, 1.642400929185890127E-16, 7.700000000000000178 ) ) ;
#11395 = ORIENTED_EDGE ( 'NONE', *, *, #17989, .F. ) ;
#11396 = CARTESIAN_POINT ( 'NONE',  ( -1.821706171509118954, -5.202118644067803999, 5.646608543709410455 ) ) ;
#11397 = B_SPLINE_CURVE_WITH_KNOTS ( 'NONE', 3,
 ( #26, #194, #15489, #2797, #8441, #14075, #11314, #4259, #2891, #8538, #13061, #4797, #6202, #11859, #4447 ),
 .UNSPECIFIED., .F., .F.,
 ( 4, 1, 1, 1, 1, 1, 1, 1, 1, 1, 1, 1, 4 ),
 ( 0.000000000000000000, 0.04238993203366740042, 0.08487769703127090448, 0.1274691104750300119, 0.1700369147469420195, 0.2126104510727770125, 0.2551841450616499918, 0.2977574123561499975, 0.3403308656859569958, 0.3829042603268439926, 0.4254776701664709782, 0.4680510765564160347, 0.4999998211434338868 ),
 .UNSPECIFIED. ) ;
#11398 = DIRECTION ( 'NONE',  ( 0.000000000000000000, -1.000000000000000000, -6.167905692361979821E-17 ) ) ;
#11399 = CARTESIAN_POINT ( 'NONE',  ( -1.899999999999999911, 2.799999999999999822, 1.600000000000000089 ) ) ;
#11400 = DIRECTION ( 'NONE',  ( -1.000000000000000000, 0.000000000000000000, 0.000000000000000000 ) ) ;
#11401 = DIRECTION ( 'NONE',  ( -6.123233995736769734E-17, 3.749399456654650178E-33, -1.000000000000000000 ) ) ;
#11402 = DIRECTION ( 'NONE',  ( -2.960594732333750117E-16, -1.000000000000000000, 0.000000000000000000 ) ) ;
#11403 = PLANE ( 'NONE',  #14455 ) ;
#11404 = CARTESIAN_POINT ( 'NONE',  ( 1.167621112247380077, -2.821367850108300157, 6.743381174846749815 ) ) ;
#11405 = CARTESIAN_POINT ( 'NONE',  ( 0.9976707306414894783, -2.522460978720530989, 6.494311833503137343 ) ) ;
#11406 = CARTESIAN_POINT ( 'NONE',  ( -1.300961508564169922, -0.1779661016949160013, 6.661123742937279602 ) ) ;
#11407 = EDGE_CURVE ( 'NONE', #3506, #12486, #4441, .T. ) ;
#11408 = CARTESIAN_POINT ( 'NONE',  ( 1.707817112497189926, -0.4112288135593229477, 6.319218296629480314 ) ) ;
#11409 = LINE ( 'NONE', #17039, #16490 ) ;
#11410 = EDGE_CURVE ( 'NONE', #16183, #3220, #4683, .T. ) ;
#11411 = CARTESIAN_POINT ( 'NONE',  ( -1.899999999999999911, 4.218847493575600080E-16, 1.163414459189990120E-16 ) ) ;
#11412 = ORIENTED_EDGE ( 'NONE', *, *, #16003, .T. ) ;
#11413 = EDGE_CURVE ( 'NONE', #9351, #11433, #7649, .T. ) ;
#11414 = CARTESIAN_POINT ( 'NONE',  ( -1.236334101859210000, -2.029566048306499670, 2.697445712080720259 ) ) ;
#11415 = VERTEX_POINT ( 'NONE', #16080 ) ;
#11416 = EDGE_CURVE ( 'NONE', #14928, #14900, #13293, .T. ) ;
#11417 = ORIENTED_EDGE ( 'NONE', *, *, #11893, .F. ) ;
#11418 = CARTESIAN_POINT ( 'NONE',  ( -1.074829861819749821, -3.314262780522329255, 2.606322265575610864 ) ) ;
#11419 = DIRECTION ( 'NONE',  ( 1.000000000000000000, 0.000000000000000000, 0.000000000000000000 ) ) ;
#11420 = CARTESIAN_POINT ( 'NONE',  ( 0.07064654565475687875, -5.448728813559320372, 7.352897294663512717 ) ) ;
#11421 = AXIS2_PLACEMENT_3D ( 'NONE', #12690, #17017, #4433 ) ;
#11422 = ORIENTED_EDGE ( 'NONE', *, *, #2983, .F. ) ;
#11423 = CARTESIAN_POINT ( 'NONE',  ( 2.012177589105479392, -0.3845338983050847759, 5.107213040360584877 ) ) ;
#11424 = ORIENTED_EDGE ( 'NONE', *, *, #13793, .F. ) ;
#11425 = CYLINDRICAL_SURFACE ( 'NONE', #13190, 0.6000000000000000888 ) ;
#11426 = CARTESIAN_POINT ( 'NONE',  ( 2.052456847059610734, -2.565196678937129438, 4.748194746458525017 ) ) ;
#11427 = CARTESIAN_POINT ( 'NONE',  ( 1.347262683220810553, -0.4245762711864407013, 6.986424775243341045 ) ) ;
#11428 = ORIENTED_EDGE ( 'NONE', *, *, #7167, .T. ) ;
#11429 = CARTESIAN_POINT ( 'NONE',  ( -1.850000000000000089, 11.25000000000000000, 8.300000000000000711 ) ) ;
#11430 = CARTESIAN_POINT ( 'NONE',  ( 0.1365430262726380628, -0.4468220338983063811, 6.748423079423377047 ) ) ;
#11431 = ADVANCED_FACE ( 'NONE', ( #4418 ), #10077, .F. ) ;
#11432 = AXIS2_PLACEMENT_3D ( 'NONE', #3349, #10934, #9541 ) ;
#11433 = VERTEX_POINT ( 'NONE', #433 ) ;
#11434 = DIRECTION ( 'NONE',  ( 1.734723475976809806E-16, -1.000000000000000000, 0.000000000000000000 ) ) ;
#11435 = CARTESIAN_POINT ( 'NONE',  ( -1.392553072310521278, -5.564406779661021041, 3.191531554476531252 ) ) ;
#11436 = DIRECTION ( 'NONE',  ( 1.000000000000000000, 1.644774851296529842E-16, 1.110223024625159992E-16 ) ) ;
#11437 = CARTESIAN_POINT ( 'NONE',  ( 1.983927814618709873E-15, 10.80000000000000071, 8.599999999999999645 ) ) ;
#11438 = CIRCLE ( 'NONE', #14140, 0.3499999999999999778 ) ;
#11439 = ORIENTED_EDGE ( 'NONE', *, *, #10619, .F. ) ;
#11440 = CARTESIAN_POINT ( 'NONE',  ( -1.899999999999999911, 10.00000000000000000, 1.600000000000000089 ) ) ;
#11441 = CARTESIAN_POINT ( 'NONE',  ( 1.465095039565329937, -2.033406924666469884, 2.858195935359850282 ) ) ;
#11442 = VECTOR ( 'NONE', #15471, 1000.000000000000000 ) ;
#11443 = ADVANCED_FACE ( 'NONE', ( #3211 ), #14509, .T. ) ;
#11444 = LINE ( 'NONE', #15719, #9343 ) ;
#11445 = AXIS2_PLACEMENT_3D ( 'NONE', #5841, #2987, #5479 ) ;
#11446 = CARTESIAN_POINT ( 'NONE',  ( -1.627161714697918704, -1.637506023765568530, 3.448102801005849649 ) ) ;
#11447 = VECTOR ( 'NONE', #17718, 1000.000000000000000 ) ;
#11448 = CARTESIAN_POINT ( 'NONE',  ( -3.061616997868380553E-17, 5.318248954186070243, 6.899999999999999467 ) ) ;
#11449 = ORIENTED_EDGE ( 'NONE', *, *, #16488, .F. ) ;
#11450 = CIRCLE ( 'NONE', #8494, 0.4000000000000000222 ) ;
#11451 = EDGE_CURVE ( 'NONE', #17532, #8938, #3113, .T. ) ;
#11452 = DIRECTION ( 'NONE',  ( 0.7071067811865470176, -0.7071067811865480168, 0.000000000000000000 ) ) ;
#11453 = CARTESIAN_POINT ( 'NONE',  ( -2.304156201936080617, -0.5002118644067795605, 6.016707707703351282 ) ) ;
#11454 = CARTESIAN_POINT ( 'NONE',  ( -0.6864473529425049181, -4.591277760018209975, 6.951118770549909343 ) ) ;
#11455 = CARTESIAN_POINT ( 'NONE',  ( 7.069631497386979886E-16, 5.131370849898479136, 5.100000000000000533 ) ) ;
#11456 = DIRECTION ( 'NONE',  ( 0.000000000000000000, 6.123233995736769734E-17, -1.000000000000000000 ) ) ;
#11457 = CARTESIAN_POINT ( 'NONE',  ( -0.9002849211310044453, -5.166525423728809407, 7.196465912290821443 ) ) ;
#11458 = EDGE_LOOP ( 'NONE', ( #17064, #2464, #2018, #8656 ) ) ;
#11459 = VECTOR ( 'NONE', #427, 1000.000000000000000 ) ;
#11460 = VERTEX_POINT ( 'NONE', #8765 ) ;
#11461 = PLANE ( 'NONE',  #6528 ) ;
#11462 = DIRECTION ( 'NONE',  ( 1.189524669241239855E-16, -1.000000000000000000, 0.000000000000000000 ) ) ;
#11463 = VERTEX_POINT ( 'NONE', #10419 ) ;
#11464 = CIRCLE ( 'NONE', #1704, 0.5000000000000000000 ) ;
#11465 = CARTESIAN_POINT ( 'NONE',  ( 1.899999999999999911, 0.8000000000000000444, -2.399999999999999911 ) ) ;
#11466 = CARTESIAN_POINT ( 'NONE',  ( 1.468674196027861756, -1.237764246504700072, 6.910454658870847311 ) ) ;
#11467 = AXIS2_PLACEMENT_3D ( 'NONE', #2923, #1533, #134 ) ;
#11468 = CARTESIAN_POINT ( 'NONE',  ( 2.500000000000000000, 4.700000000000000178, 0.5999999999999999778 ) ) ;
#11469 = LINE ( 'NONE', #534, #14684 ) ;
#11470 = CARTESIAN_POINT ( 'NONE',  ( -0.1768565782246520057, -1.847100618360170143, 2.353200596935780098 ) ) ;
#11471 = CARTESIAN_POINT ( 'NONE',  ( -2.500000000000000000, 2.799999999999999822, 1.600000000000000089 ) ) ;
#11472 = CIRCLE ( 'NONE', #1130, 0.4000000000000001887 ) ;
#11473 = CARTESIAN_POINT ( 'NONE',  ( 2.190084968185480374, -4.032358841099290103, 3.838447030292440054 ) ) ;
#11474 = EDGE_CURVE ( 'NONE', #8434, #10381, #14323, .T. ) ;
#11475 = CARTESIAN_POINT ( 'NONE',  ( 0.3509990757148593321, -4.474836318576761229, 6.722795464567642654 ) ) ;
#11476 = PLANE ( 'NONE',  #3482 ) ;
#11477 = CARTESIAN_POINT ( 'NONE',  ( 2.116444151961470066, -0.3533898305084750002, 3.670839500609349937 ) ) ;
#11478 = VECTOR ( 'NONE', #623, 1000.000000000000000 ) ;
#11479 = DIRECTION ( 'NONE',  ( -1.000000000000000000, 0.000000000000000000, 0.000000000000000000 ) ) ;
#11480 = ORIENTED_EDGE ( 'NONE', *, *, #16707, .T. ) ;
#11481 = VECTOR ( 'NONE', #15116, 1000.000000000000000 ) ;
#11482 = DIRECTION ( 'NONE',  ( 0.000000000000000000, -1.000000000000000000, 0.000000000000000000 ) ) ;
#11483 = ORIENTED_EDGE ( 'NONE', *, *, #14270, .T. ) ;
#11484 = DIRECTION ( 'NONE',  ( 1.000000000000000000, 1.233581138472399909E-16, 1.480297366166879989E-16 ) ) ;
#11485 = EDGE_CURVE ( 'NONE', #5242, #6826, #17144, .T. ) ;
#11486 = CIRCLE ( 'NONE', #6151, 0.3499999999999996447 ) ;
#11487 = ORIENTED_EDGE ( 'NONE', *, *, #13318, .F. ) ;
#11488 = CARTESIAN_POINT ( 'NONE',  ( 0.4339619423229844619, -5.439830508474575943, 6.706578715862737461 ) ) ;
#11489 = CARTESIAN_POINT ( 'NONE',  ( -1.818868030982659700, -3.244397915657463827, 2.767428454397828919 ) ) ;
#11490 = DIRECTION ( 'NONE',  ( 0.000000000000000000, 1.000000000000000000, 0.000000000000000000 ) ) ;
#11491 = VECTOR ( 'NONE', #13905, 1000.000000000000000 ) ;
#11492 = DIRECTION ( 'NONE',  ( -6.162975822039159109E-32, -1.000000000000000000, -1.110223024625159992E-16 ) ) ;
#11493 = AXIS2_PLACEMENT_3D ( 'NONE', #3136, #8791, #17197 ) ;
#11494 = CARTESIAN_POINT ( 'NONE',  ( -1.364983921886200546, -4.865515740159335856, 2.403349116468209257 ) ) ;
#11495 = FACE_OUTER_BOUND ( 'NONE', #13346, .T. ) ;
#11496 = DIRECTION ( 'NONE',  ( -1.000000000000000000, 0.000000000000000000, 0.000000000000000000 ) ) ;
#11497 = CARTESIAN_POINT ( 'NONE',  ( -1.332058588847369940, -3.100827309567760537, 6.640197310420220767 ) ) ;
#11498 = CARTESIAN_POINT ( 'NONE',  ( 2.021195349941390162, -3.780028546288090041, 4.339901124684640621 ) ) ;
#11499 = CARTESIAN_POINT ( 'NONE',  ( 1.526871680339569659, -0.04004237288135625850, 3.327650196883443101 ) ) ;
#11500 =( GEOMETRIC_REPRESENTATION_CONTEXT ( 3 ) GLOBAL_UNCERTAINTY_ASSIGNED_CONTEXT ( ( #15300 ) ) GLOBAL_UNIT_ASSIGNED_CONTEXT ( ( #1243, #5322, #16613 ) ) REPRESENTATION_CONTEXT ( 'NONE', 'WORKASPACE' ) );
#11501 = CARTESIAN_POINT ( 'NONE',  ( -0.008736317425858650815, -5.288463233533899910, 2.411138844410889881 ) ) ;
#11502 = DIRECTION ( 'NONE',  ( 0.000000000000000000, -1.000000000000000000, 0.000000000000000000 ) ) ;
#11503 = ORIENTED_EDGE ( 'NONE', *, *, #14242, .F. ) ;
#11504 =( BOUNDED_SURFACE ( )  B_SPLINE_SURFACE ( 3, 3, ( 
 ( #13913, #2620, #7161, #1227, #4177, #7241, #12798 ),
 ( #5759, #6871, #17032, #16683, #14355, #8710, #1677 ),
 ( #15759, #5843, #11494, #17125, #12882, #3067, #196 ),
 ( #4449, #10108, #3546, #9193, #16240, #12263, #11982 ),
 ( #17881, #1156, #17790, #13563, #14855, #10777, #15145 ),
 ( #4932, #967, #17981, #5127, #8103, #10587, #17595 ),
 ( #5326, #12173, #16618, #15232, #3918, #10688, #9574 ) ),
 .UNSPECIFIED., .T., .F., .F. ) 
 B_SPLINE_SURFACE_WITH_KNOTS ( ( 4, 3, 4 ),
 ( 4, 1, 1, 1, 4 ),
 ( 0.000000000000000000, 3.141592653589790007, 6.283185307179590673 ),
 ( 18.06415775814129887, 18.36448856483159986, 18.49670707487869947, 18.62179267666130045, 18.84955592153880133 ),
 .UNSPECIFIED. ) 
 GEOMETRIC_REPRESENTATION_ITEM ( )  RATIONAL_B_SPLINE_SURFACE ( (
 ( 1.000000000000000000, 1.000000000000000000, 1.000000000000000000, 1.000000000000000000, 1.000000000000000000, 1.000000000000000000, 1.000000000000000000),
 ( 0.3333333333333329818, 0.3333333333333329818, 0.3333333333333329818, 0.3333333333333329818, 0.3333333333333329818, 0.3333333333333329818, 0.3333333333333329818),
 ( 0.3333333333333329818, 0.3333333333333329818, 0.3333333333333329818, 0.3333333333333329818, 0.3333333333333329818, 0.3333333333333329818, 0.3333333333333329818),
 ( 1.000000000000000000, 1.000000000000000000, 1.000000000000000000, 1.000000000000000000, 1.000000000000000000, 1.000000000000000000, 1.000000000000000000),
 ( 0.3333333333333329818, 0.3333333333333329818, 0.3333333333333329818, 0.3333333333333329818, 0.3333333333333329818, 0.3333333333333329818, 0.3333333333333329818),
 ( 0.3333333333333329818, 0.3333333333333329818, 0.3333333333333329818, 0.3333333333333329818, 0.3333333333333329818, 0.3333333333333329818, 0.3333333333333329818),
 ( 1.000000000000000000, 1.000000000000000000, 1.000000000000000000, 1.000000000000000000, 1.000000000000000000, 1.000000000000000000, 1.000000000000000000) ) ) 
 REPRESENTATION_ITEM ( '' )  SURFACE ( )  );
#11505 = CARTESIAN_POINT ( 'NONE',  ( -2.286166334984490067, -0.2135593220338989906, 5.258525443163870605 ) ) ;
#11506 = CARTESIAN_POINT ( 'NONE',  ( -2.091095264232510242, -1.656953435693890198, 5.779845490516250628 ) ) ;
#11507 = EDGE_LOOP ( 'NONE', ( #15187, #7989, #10506, #12941, #8729, #14812, #7620, #16498, #353, #11617, #10155, #18109, #9872, #18040, #10011, #6289, #18272, #15134, #7991, #6739, #9733, #258, #15393, #5102, #13637, #1892, #18141, #17093 ) ) ;
#11508 = VECTOR ( 'NONE', #554, 1000.000000000000000 ) ;
#11509 = EDGE_LOOP ( 'NONE', ( #15496, #9824, #13533, #3162 ) ) ;
#11510 = CARTESIAN_POINT ( 'NONE',  ( 2.267872052190589738, -3.756740257999800825, 4.071110468860601017 ) ) ;
#11511 = CARTESIAN_POINT ( 'NONE',  ( 2.431060148753489081, -5.055296610169490279, 3.635668498923322112 ) ) ;
#11512 = ORIENTED_EDGE ( 'NONE', *, *, #2622, .T. ) ;
#11513 = EDGE_CURVE ( 'NONE', #9201, #10948, #16440, .T. ) ;
#11514 = CARTESIAN_POINT ( 'NONE',  ( -1.449568901432419343, -0.5625000000000005551, 3.250431098567584165 ) ) ;
#11515 = ORIENTED_EDGE ( 'NONE', *, *, #582, .F. ) ;
#11516 = EDGE_CURVE ( 'NONE', #2878, #1367, #2086, .T. ) ;
#11517 = DIRECTION ( 'NONE',  ( 0.000000000000000000, 6.055990775824630636E-30, -1.000000000000000000 ) ) ;
#11518 = CARTESIAN_POINT ( 'NONE',  ( 1.399999999999999911, -8.000000000000000000, 6.100000000000000533 ) ) ;
#11519 = ADVANCED_FACE ( 'NONE', ( #3466 ), #13754, .T. ) ;
#11520 = VECTOR ( 'NONE', #4721, 1000.000000000000000 ) ;
#11521 = CARTESIAN_POINT ( 'NONE',  ( 1.928470600873580132, -2.472043525783979678, 3.995796205495612874 ) ) ;
#11522 = ORIENTED_EDGE ( 'NONE', *, *, #6088, .T. ) ;
#11523 = LINE ( 'NONE', #17151, #11905 ) ;
#11524 = LINE ( 'NONE', #4474, #4919 ) ;
#11525 = ORIENTED_EDGE ( 'NONE', *, *, #7553, .F. ) ;
#11526 = CARTESIAN_POINT ( 'NONE',  ( -0.009452017499193299602, -0.5998064736617420012, 2.336684903355690235 ) ) ;
#11527 = CARTESIAN_POINT ( 'NONE',  ( 0.7982439214406963357, -5.430932203389830626, 6.591424794228156081 ) ) ;
#11528 = CARTESIAN_POINT ( 'NONE',  ( -2.286166334984490067, -0.2135593220338989628, 5.258525443163869717 ) ) ;
#11529 = AXIS2_PLACEMENT_3D ( 'NONE', #15370, #2576, #9610 ) ;
#11530 = CARTESIAN_POINT ( 'NONE',  ( -1.899999999999999911, 11.15000000000000036, 1.600000000000000089 ) ) ;
#11531 = ORIENTED_EDGE ( 'NONE', *, *, #5108, .F. ) ;
#11532 = LINE ( 'NONE', #9787, #1108 ) ;
#11533 = CARTESIAN_POINT ( 'NONE',  ( -2.100188519621619676, -1.590929447189000090, 3.637948273607420013 ) ) ;
#11534 = EDGE_CURVE ( 'NONE', #6673, #12793, #17900, .T. ) ;
#11535 = CARTESIAN_POINT ( 'NONE',  ( 2.500000000000000000, 11.29999999999999893, 7.649999999999999467 ) ) ;
#11536 = CARTESIAN_POINT ( 'NONE',  ( -0.8493734496527890476, -2.755343861603408939, 6.569081749323187225 ) ) ;
#11537 = DIRECTION ( 'NONE',  ( -2.220446049250309876E-16, 0.000000000000000000, 1.000000000000000000 ) ) ;
#11538 = ORIENTED_EDGE ( 'NONE', *, *, #13276, .F. ) ;
#11539 = VECTOR ( 'NONE', #698, 1000.000000000000000 ) ;
#11540 = CARTESIAN_POINT ( 'NONE',  ( 2.500000000000000000, 7.299999999999999822, 1.600000000000000089 ) ) ;
#11541 = CARTESIAN_POINT ( 'NONE',  ( 1.255262969126039558E-16, -2.775557561562890858E-16, 2.050000000000001155 ) ) ;
#11542 = CARTESIAN_POINT ( 'NONE',  ( -1.777964140657649850, -4.731007489747940831, 6.241943319976260618 ) ) ;
#11543 = LINE ( 'NONE', #6250, #11933 ) ;
#11544 = LINE ( 'NONE', #520, #9162 ) ;
#11545 = CARTESIAN_POINT ( 'NONE',  ( -1.192209327851089240, -5.277754237288146300, 2.329031440774910422 ) ) ;
#11546 = VERTEX_POINT ( 'NONE', #15160 ) ;
#11547 = EDGE_LOOP ( 'NONE', ( #4819, #8092, #17025, #5592 ) ) ;
#11548 = DIRECTION ( 'NONE',  ( 1.000000000000000000, 0.000000000000000000, 0.000000000000000000 ) ) ;
#11549 = DIRECTION ( 'NONE',  ( -6.123233995736769734E-17, 0.000000000000000000, -1.000000000000000000 ) ) ;
#11550 = ORIENTED_EDGE ( 'NONE', *, *, #13326, .F. ) ;
#11551 = ADVANCED_FACE ( 'NONE', ( #5143 ), #10607, .T. ) ;
#11552 = CARTESIAN_POINT ( 'NONE',  ( -2.235075160050040921, -1.633665147405598761, 6.130927224539796327 ) ) ;
#11553 = EDGE_CURVE ( 'NONE', #2341, #16759, #10794, .T. ) ;
#11554 = LINE ( 'NONE', #443, #15329 ) ;
#11555 = DIRECTION ( 'NONE',  ( 1.000000000000000000, 0.000000000000000000, 0.000000000000000000 ) ) ;
#11556 = VECTOR ( 'NONE', #1292, 1000.000000000000000 ) ;
#11557 = CARTESIAN_POINT ( 'NONE',  ( 0.4790341583531380065, -1.916965483225030242, 2.395814251711720022 ) ) ;
#11558 = CARTESIAN_POINT ( 'NONE',  ( 1.104321075428930765, -5.320452325212860600, 2.282937282173381099 ) ) ;
#11559 = CARTESIAN_POINT ( 'NONE',  ( -2.603140590302631008, -1.726818300558751851, 5.216500493824310247 ) ) ;
#11560 = DIRECTION ( 'NONE',  ( -1.000000000000000000, 0.000000000000000000, 0.000000000000000000 ) ) ;
#11561 = CARTESIAN_POINT ( 'NONE',  ( -1.990095963740230900, -4.847448931189385135, 5.204400533041805943 ) ) ;
#11562 = CARTESIAN_POINT ( 'NONE',  ( -0.5500000000000000444, 6.450000000000000178, 3.399999999999999911 ) ) ;
#11563 = DIRECTION ( 'NONE',  ( 0.000000000000000000, -1.000000000000000000, -1.769136588914770194E-30 ) ) ;
#11564 = ORIENTED_EDGE ( 'NONE', *, *, #7147, .F. ) ;
#11565 = FILL_AREA_STYLE_COLOUR ( '', #18126 ) ;
#11566 = EDGE_LOOP ( 'NONE', ( #4468, #7803, #14264, #5926, #441, #12701, #15221, #12250, #11023, #16939, #18213, #10422, #7932, #6794, #1818, #9112, #4079, #17244, #8758, #4677, #657, #10421, #11718, #17724 ) ) ;
#11567 = CARTESIAN_POINT ( 'NONE',  ( 1.000000000000000000, 6.799999999999999822, 7.700000000000000178 ) ) ;
#11568 = ORIENTED_EDGE ( 'NONE', *, *, #6540, .T. ) ;
#11569 = EDGE_CURVE ( 'NONE', #5150, #6699, #4953, .T. ) ;
#11570 = CARTESIAN_POINT ( 'NONE',  ( -0.3265524029357583236, -5.457627118644064801, 6.726831181542982208 ) ) ;
#11571 = CARTESIAN_POINT ( 'NONE',  ( -1.991177874369409961, -3.221109627369172390, 2.945484578117480989 ) ) ;
#11572 = EDGE_CURVE ( 'NONE', #4524, #14928, #20, .T. ) ;
#11573 = LINE ( 'NONE', #11665, #13494 ) ;
#11574 = DIRECTION ( 'NONE',  ( -2.220446049250309876E-16, -1.000000000000000000, 5.551115123125800057E-15 ) ) ;
#11575 = FACE_OUTER_BOUND ( 'NONE', #13507, .T. ) ;
#11576 = CARTESIAN_POINT ( 'NONE',  ( 1.353103843060669886, -2.798079561820010053, 6.625579309552930063 ) ) ;
#11577 = CARTESIAN_POINT ( 'NONE',  ( 1.823404397755048700, -3.943046564306109669, 5.643450181448720571 ) ) ;
#11578 =( REPRESENTATION_RELATIONSHIP ('NONE','NONE', #2757, #5932 ) REPRESENTATION_RELATIONSHIP_WITH_TRANSFORMATION ( #577 )SHAPE_REPRESENTATION_RELATIONSHIP( ) );
#11579 = CARTESIAN_POINT ( 'NONE',  ( -2.328217775191430139, -0.2180084745762720100, 5.043379051721170292 ) ) ;
#11580 = PLANE ( 'NONE',  #2900 ) ;
#11581 = CARTESIAN_POINT ( 'NONE',  ( -2.034805890357269220, -0.5313559322033900578, 4.427518626519226785 ) ) ;
#11582 = CARTESIAN_POINT ( 'NONE',  ( -0.7500000000000000000, 6.450000000000000178, 2.699264068711930253 ) ) ;
#11583 = ORIENTED_EDGE ( 'NONE', *, *, #2705, .T. ) ;
#11584 = CARTESIAN_POINT ( 'NONE',  ( 2.461935615161780611, -3.919758276017824006, 5.690952430644305338 ) ) ;
#11585 = CARTESIAN_POINT ( 'NONE',  ( 2.022304719220918479, -0.06673728813559356987, 4.346496488058688712 ) ) ;
#11586 = CARTESIAN_POINT ( 'NONE',  ( 0.8748826269292639957, -2.262448931189380286, 2.515205712983200392 ) ) ;
#11587 = ORIENTED_EDGE ( 'NONE', *, *, #5871, .F. ) ;
#11588 = DIRECTION ( 'NONE',  ( 0.000000000000000000, -1.000000000000000000, -6.167905692361979821E-17 ) ) ;
#11589 = VERTEX_POINT ( 'NONE', #9303 ) ;
#11590 = CARTESIAN_POINT ( 'NONE',  ( 1.044181395669779633, -3.547145663405210314, 2.590869634085890993 ) ) ;
#11591 = EDGE_CURVE ( 'NONE', #4320, #12426, #6621, .T. ) ;
#11592 = PRODUCT_CONTEXT ( 'NONE', #5912, 'mechanical' ) ;
#11593 = CARTESIAN_POINT ( 'NONE',  ( 1.873832970144350130, -5.037500000000000533, 2.826167029855650270 ) ) ;
#11594 = FACE_OUTER_BOUND ( 'NONE', #546, .T. ) ;
#11595 = VECTOR ( 'NONE', #18198, 1000.000000000000000 ) ;
#11596 = VERTEX_POINT ( 'NONE', #4857 ) ;
#11597 = LINE ( 'NONE', #6128, #11759 ) ;
#11598 = CARTESIAN_POINT ( 'NONE',  ( 0.5999999999999999778, 11.40000000000000036, 7.599999999999999645 ) ) ;
#11599 = ORIENTED_EDGE ( 'NONE', *, *, #7896, .F. ) ;
#11600 = CARTESIAN_POINT ( 'NONE',  ( -0.5999999999999999778, 0.5999999999999999778, 7.700000000000000178 ) ) ;
#11601 = CARTESIAN_POINT ( 'NONE',  ( -0.4625564304287554940, -3.007674156414608557, 6.700235833919871986 ) ) ;
#11602 = LINE ( 'NONE', #10129, #16185 ) ;
#11603 = CARTESIAN_POINT ( 'NONE',  ( -1.661700935788390066, -0.5625000000000000000, 3.038299064211610112 ) ) ;
#11604 = EDGE_LOOP ( 'NONE', ( #2550, #16278, #9408, #1849, #6629, #11128 ) ) ;
#11605 = PLANE ( 'NONE',  #8659 ) ;
#11606 = CARTESIAN_POINT ( 'NONE',  ( 2.500000000000000000, 7.299999999999999822, 0.5999999999999999778 ) ) ;
#11607 = LINE ( 'NONE', #9348, #15346 ) ;
#11608 = EDGE_LOOP ( 'NONE', ( #9632, #15524, #6123, #14530 ) ) ;
#11609 = DIRECTION ( 'NONE',  ( 0.000000000000000000, 1.000000000000000000, 0.000000000000000000 ) ) ;
#11610 = CARTESIAN_POINT ( 'NONE',  ( -0.8731223871104993872, -5.470974576271190770, 6.558046933601121786 ) ) ;
#11611 = DIRECTION ( 'NONE',  ( 0.000000000000000000, 0.000000000000000000, 1.000000000000000000 ) ) ;
#11612 = EDGE_CURVE ( 'NONE', #10192, #9205, #5028, .T. ) ;
#11613 = VECTOR ( 'NONE', #2072, 1000.000000000000000 ) ;
#11614 = CARTESIAN_POINT ( 'NONE',  ( -2.332582362116870200, -0.2313559322033900412, 4.387643303570821551 ) ) ;
#11615 = EDGE_CURVE ( 'NONE', #14464, #6674, #3542, .T. ) ;
#11616 = CARTESIAN_POINT ( 'NONE',  ( -0.2908063684825371031, -4.544701183441625325, 7.337905485238597869 ) ) ;
#11617 = ORIENTED_EDGE ( 'NONE', *, *, #16963, .T. ) ;
#11618 = CARTESIAN_POINT ( 'NONE',  ( 2.219956784870649624, -2.173136654396199852, 3.918630970161570026 ) ) ;
#11619 = DIRECTION ( 'NONE',  ( -2.220446049250309876E-16, 0.000000000000000000, 1.000000000000000000 ) ) ;
#11620 = CARTESIAN_POINT ( 'NONE',  ( 1.883235269974540937, -2.359442960702510472, 5.517512544583896172 ) ) ;
#11621 = DIRECTION ( 'NONE',  ( 0.000000000000000000, -1.836189155707839943E-31, -1.000000000000000000 ) ) ;
#11622 = DIRECTION ( 'NONE',  ( 0.7071067811865594521, 0.000000000000000000, 0.7071067811865355823 ) ) ;
#11623 = ORIENTED_EDGE ( 'NONE', *, *, #1552, .F. ) ;
#11624 = EDGE_CURVE ( 'NONE', #4443, #4993, #16544, .T. ) ;
#11625 = CARTESIAN_POINT ( 'NONE',  ( 1.000000000000000000, -5.599999999999999645, 5.100000000000000533 ) ) ;
#11626 = CARTESIAN_POINT ( 'NONE',  ( 2.632587027711251526, -0.6593979156574641953, 4.364441905910536157 ) ) ;
#11627 = CARTESIAN_POINT ( 'NONE',  ( -2.161802606005209793, -5.010466949207389220, 3.769755311421840283 ) ) ;
#11628 = CARTESIAN_POINT ( 'NONE',  ( 1.889999999999999902, 4.700000000000000178, -4.702461056355109900E-16 ) ) ;
#11629 = DIRECTION ( 'NONE',  ( 0.000000000000000000, -1.000000000000000000, 0.000000000000000000 ) ) ;
#11630 = CARTESIAN_POINT ( 'NONE',  ( -0.2469343877495291661, -5.295550847457634269, 2.057675570509529539 ) ) ;
#11631 = ORIENTED_EDGE ( 'NONE', *, *, #2132, .F. ) ;
#11632 = ADVANCED_FACE ( 'NONE', ( #6334 ), #3852, .F. ) ;
#11633 = ORIENTED_EDGE ( 'NONE', *, *, #3297, .T. ) ;
#11634 = DIRECTION ( 'NONE',  ( -1.000000000000000000, 1.224646799147350002E-16, 0.000000000000000000 ) ) ;
#11635 = ADVANCED_FACE ( 'NONE', ( #9208 ), #12190, .T. ) ;
#11636 = SHAPE_REPRESENTATION_RELATIONSHIP ( 'NONE' , 'NONE' ,  #853, #11297 ) ;
#11637 = LINE ( 'NONE', #3218, #3747 ) ;
#11638 = ADVANCED_FACE ( 'NONE', ( #17720 ), #8900, .T. ) ;
#11639 = EDGE_LOOP ( 'NONE', ( #10098, #9118, #15675, #12282 ) ) ;
#11640 = CARTESIAN_POINT ( 'NONE',  ( -2.033393610350109793, -4.777584066324510381, 5.884928737465370041 ) ) ;
#11641 = PLANE ( 'NONE',  #3785 ) ;
#11642 = CARTESIAN_POINT ( 'NONE',  ( -8.878689293818279999E-17, 6.750000000000000000, 6.300000000000002487 ) ) ;
#11643 = CARTESIAN_POINT ( 'NONE',  ( -1.353103843060629918, -2.801920438179979822, 6.625579309552960261 ) ) ;
#11644 = CARTESIAN_POINT ( 'NONE',  ( -0.009452110982655139229, -5.299807955295460005, 2.350000000000000089 ) ) ;
#11645 = CARTESIAN_POINT ( 'NONE',  ( -2.334748642087669523, -4.940602084342530453, 4.403867486184871005 ) ) ;
#11646 = VECTOR ( 'NONE', #9732, 1000.000000000000000 ) ;
#11647 = DIRECTION ( 'NONE',  ( -1.762990951819940286E-17, -1.000000000000000000, -2.891205793294679017E-15 ) ) ;
#11648 = CARTESIAN_POINT ( 'NONE',  ( 1.803891155489780074, -0.8185750573155089471, 3.188470185434109982 ) ) ;
#11649 = CARTESIAN_POINT ( 'NONE',  ( -2.286166334984490067, -0.5135593220338989795, 5.258525443163870605 ) ) ;
#11650 = DIRECTION ( 'NONE',  ( 1.000000000000000000, 0.000000000000000000, 0.000000000000000000 ) ) ;
#11651 = CARTESIAN_POINT ( 'NONE',  ( 0.3367924244280819934, 2.254758922476410188, 8.300000000000000711 ) ) ;
#11652 = VERTEX_POINT ( 'NONE', #2748 ) ;
#11653 = EDGE_CURVE ( 'NONE', #15319, #7510, #15624, .T. ) ;
#11654 = CARTESIAN_POINT ( 'NONE',  ( -0.1749999999999999889, 7.900000000000000355, 0.5999999999999999778 ) ) ;
#11655 = VERTEX_POINT ( 'NONE', #17996 ) ;
#11656 = PLANE ( 'NONE',  #803 ) ;
#11657 = B_SPLINE_CURVE_WITH_KNOTS ( 'NONE', 3,
 ( #6462, #3589, #2575, #15184, #9437, #13875, #921, #11004, #5076, #10815, #6559, #16566, #16463, #17830, #5268 ),
 .UNSPECIFIED., .F., .F.,
 ( 4, 1, 1, 1, 1, 1, 1, 1, 1, 1, 1, 1, 4 ),
 ( 0.000000000000000000, 0.04238384222883789798, 0.08486641011426379611, 0.1274541364341190142, 0.1700199979528400074, 0.2125927824332390081, 0.2551660849076620163, 0.2977383825899770353, 0.3403095086483710063, 0.3828788202030369847, 0.4254464832354110104, 0.4680130360807339684, 0.4999998212288473409 ),
 .UNSPECIFIED. ) ;
#11658 = CARTESIAN_POINT ( 'NONE',  ( -1.889999999999999902, 8.500000000000000000, 0.6099999999999999867 ) ) ;
#11659 = ORIENTED_EDGE ( 'NONE', *, *, #6195, .F. ) ;
#11660 = CARTESIAN_POINT ( 'NONE',  ( -0.1365430262726299304, -5.453177966101685037, 6.748423079423377047 ) ) ;
#11661 = LINE ( 'NONE', #2025, #6460 ) ;
#11662 = CARTESIAN_POINT ( 'NONE',  ( -2.619177996481920179, -3.081379897639443310, 4.272191262657214494 ) ) ;
#11663 = DIRECTION ( 'NONE',  ( 1.000000000000000000, -2.220446049250309876E-16, -6.049014748177260544E-16 ) ) ;
#11664 = CARTESIAN_POINT ( 'NONE',  ( 0.1749999999999999889, 8.200000000000001066, -3.200000000000000178 ) ) ;
#11665 = CARTESIAN_POINT ( 'NONE',  ( -1.899999999999999911, -2.607830583485260225E-17, -8.881784197001250351E-16 ) ) ;
#11666 = B_SPLINE_CURVE_WITH_KNOTS ( 'NONE', 3,
 ( #14697, #10636, #6647, #5364, #16374, #13776, #12022 ),
 .UNSPECIFIED., .F., .F.,
 ( 4, 1, 1, 1, 4 ),
 ( 5.497787143782139729, 5.798117950472390092, 5.930336460519450625, 6.055422062302069364, 6.283185307179590673 ),
 .UNSPECIFIED. ) ;
#11667 = ADVANCED_FACE ( 'NONE', ( #9870 ), #6721, .T. ) ;
#11668 = CARTESIAN_POINT ( 'NONE',  ( -0.5902886515192680150, -1.447358841099289917, 6.978224088050050788 ) ) ;
#11669 = LINE ( 'NONE', #14791, #12691 ) ;
#11670 = CARTESIAN_POINT ( 'NONE',  ( -2.033393610350109793, -4.777584066324510381, 5.884928737465370041 ) ) ;
#11671 = CARTESIAN_POINT ( 'NONE',  ( -2.050994839075679366, -4.618406924666464519, 4.608774933727191048 ) ) ;
#11672 = CARTESIAN_POINT ( 'NONE',  ( 0.006176317641843490427, -5.052110595307439667, 2.465914288053609571 ) ) ;
#11673 = CARTESIAN_POINT ( 'NONE',  ( -1.899999999999999911, 4.700000000000000178, 1.600000000000000089 ) ) ;
#11674 = EDGE_LOOP ( 'NONE', ( #1606, #1987, #12286, #10510, #6362, #15907, #10439, #15136 ) ) ;
#11675 = CARTESIAN_POINT ( 'NONE',  ( -0.06913820924137326074, -4.222506023765566496, 7.352985789827153340 ) ) ;
#11676 = EDGE_CURVE ( 'NONE', #16660, #2436, #13915, .T. ) ;
#11677 = CARTESIAN_POINT ( 'NONE',  ( 1.622657008870240762E-16, -0.3000000000000002665, 2.649999999999998579 ) ) ;
#11678 = CARTESIAN_POINT ( 'NONE',  ( -0.4201920264140019956, -2.122719201459649874, 2.384360920086639801 ) ) ;
#11679 = ORIENTED_EDGE ( 'NONE', *, *, #4349, .T. ) ;
#11680 = ORIENTED_EDGE ( 'NONE', *, *, #13100, .T. ) ;
#11681 = CARTESIAN_POINT ( 'NONE',  ( -1.399999999999999911, 0.5999999999999999778, 6.100000000000000533 ) ) ;
#11682 = EDGE_LOOP ( 'NONE', ( #12655, #3340, #3630, #8346 ) ) ;
#11683 = CARTESIAN_POINT ( 'NONE',  ( -2.347833536521260367, -3.058091609351149653, 4.537447324629908962 ) ) ;
#11684 = DIRECTION ( 'NONE',  ( 0.000000000000000000, 0.000000000000000000, 1.000000000000000000 ) ) ;
#11685 = CARTESIAN_POINT ( 'NONE',  ( -1.747582379783008788, -5.184322033898315141, 6.697200745122486865 ) ) ;
#11686 = ORIENTED_EDGE ( 'NONE', *, *, #5628, .F. ) ;
#11687 = CARTESIAN_POINT ( 'NONE',  ( 1.899999999999999911, 3.500000000000000000, 0.6099999999999999867 ) ) ;
#11688 = CARTESIAN_POINT ( 'NONE',  ( 1.549742865090599997, -0.4156779661016959948, 6.471102547561449647 ) ) ;
#11689 = ORIENTED_EDGE ( 'NONE', *, *, #16019, .F. ) ;
#11690 = CARTESIAN_POINT ( 'NONE',  ( -1.889999999999999902, 4.100000000000000533, 3.000000000000000000 ) ) ;
#11691 = DIRECTION ( 'NONE',  ( 0.000000000000000000, 1.000000000000000000, 0.000000000000000000 ) ) ;
#11692 = CARTESIAN_POINT ( 'NONE',  ( 1.500000000000000000, -6.000000000000000000, 2.299999999999999822 ) ) ;
#11693 = CARTESIAN_POINT ( 'NONE',  ( 2.007801995112640903, -2.611773255513701653, 5.128524201241654978 ) ) ;
#11694 = CARTESIAN_POINT ( 'NONE',  ( 2.560337424259670591, -0.06228813559322075172, 4.001768473655590519 ) ) ;
#11695 = ORIENTED_EDGE ( 'NONE', *, *, #18282, .F. ) ;
#11696 = CARTESIAN_POINT ( 'NONE',  ( 0.5500000000000000444, 2.050000000000000266, 3.600000000000000089 ) ) ;
#11697 = CARTESIAN_POINT ( 'NONE',  ( -0.8740908734716290596, 4.154758922476410099, 7.700000000000000178 ) ) ;
#11698 = VERTEX_POINT ( 'NONE', #1446 ) ;
#11699 = LINE ( 'NONE', #10213, #15108 ) ;
#11700 = CARTESIAN_POINT ( 'NONE',  ( 1.477796163681079911, -5.417584745762709986, 6.531563725478140015 ) ) ;
#11701 = VECTOR ( 'NONE', #13136, 1000.000000000000000 ) ;
#11702 = DIRECTION ( 'NONE',  ( -1.000000000000000000, 0.000000000000000000, 0.000000000000000000 ) ) ;
#11703 = EDGE_CURVE ( 'NONE', #2916, #16779, #5342, .T. ) ;
#11704 = CARTESIAN_POINT ( 'NONE',  ( -2.409576349373780513, -3.450151633892079239, 3.587770028483140194 ) ) ;
#11705 = EDGE_LOOP ( 'NONE', ( #9024, #10267, #9078, #7156 ) ) ;
#11706 = CARTESIAN_POINT ( 'NONE',  ( -2.301223891756910334, -2.988226744486289999, 5.193066210047999398 ) ) ;
#11707 = CARTESIAN_POINT ( 'NONE',  ( 0.5372984490435490645, 4.599999999999999645, 8.300000000000000711 ) ) ;
#11708 = DIRECTION ( 'NONE',  ( 2.220446049250319983E-16, 0.000000000000000000, 1.000000000000000000 ) ) ;
#11709 = CARTESIAN_POINT ( 'NONE',  ( 1.865240315818150973, -2.149848366107909303, 3.842223568244794496 ) ) ;
#11710 = DIRECTION ( 'NONE',  ( 0.000000000000000000, -1.000000000000000000, 0.000000000000000000 ) ) ;
#11711 = DIRECTION ( 'NONE',  ( -4.318427418585891014E-15, 2.220446049250309876E-16, -1.000000000000000000 ) ) ;
#11712 = VECTOR ( 'NONE', #1249, 1000.000000000000000 ) ;
#11713 = ORIENTED_EDGE ( 'NONE', *, *, #8895, .T. ) ;
#11714 = EDGE_CURVE ( 'NONE', #12160, #3824, #8927, .T. ) ;
#11715 = LINE ( 'NONE', #16074, #235 ) ;
#11716 = CARTESIAN_POINT ( 'NONE',  ( 0.2254033459420760055, -0.6247245358507570456, 2.348900562125120217 ) ) ;
#11717 = CARTESIAN_POINT ( 'NONE',  ( -2.247144151254851341, -1.614217735477279536, 3.288101683376949413 ) ) ;
#11718 = ORIENTED_EDGE ( 'NONE', *, *, #13830, .T. ) ;
#11719 = CARTESIAN_POINT ( 'NONE',  ( 1.219286470748990103, -4.381683165423610582, 6.712979431025659416 ) ) ;
#11720 = LINE ( 'NONE', #4574, #13677 ) ;
#11721 = CARTESIAN_POINT ( 'NONE',  ( 7.233457020361919865E-16, 4.000000000000000000, 5.100000000000000533 ) ) ;
#11722 = CARTESIAN_POINT ( 'NONE',  ( -1.407651048079459288, -5.273305084745764759, 2.450250343405070641 ) ) ;
#11723 = ORIENTED_EDGE ( 'NONE', *, *, #10848, .F. ) ;
#11724 = ORIENTED_EDGE ( 'NONE', *, *, #12538, .F. ) ;
#11725 = CARTESIAN_POINT ( 'NONE',  ( -0.5921572875253819923, 6.450000000000000178, 1.600000000000000089 ) ) ;
#11726 = SHAPE_REPRESENTATION_RELATIONSHIP ( 'NONE' , 'NONE' ,  #4614, #686 ) ;
#11727 = CARTESIAN_POINT ( 'NONE',  ( 2.500000000000000000, 0.4000000000000000222, -2.399999999999999911 ) ) ;
#11728 = ORIENTED_EDGE ( 'NONE', *, *, #417, .F. ) ;
#11729 = VECTOR ( 'NONE', #11295, 1000.000000000000000 ) ;
#11730 = ADVANCED_FACE ( 'NONE', ( #7532 ), #15709, .T. ) ;
#11731 = CARTESIAN_POINT ( 'NONE',  ( 1.836970198721020197E-17, 2.600000000000000089, 7.700000000000000178 ) ) ;
#11732 = CARTESIAN_POINT ( 'NONE',  ( 1.630703155447489561, -2.332313796054251487, 2.606218513833050920 ) ) ;
#11733 = EDGE_CURVE ( 'NONE', #1039, #1367, #1627, .T. ) ;
#11734 = CARTESIAN_POINT ( 'NONE',  ( 1.327748599278330000, -0.4480353997208159633, 2.745754414290000334 ) ) ;
#11735 = DIRECTION ( 'NONE',  ( 0.000000000000000000, 0.000000000000000000, -1.000000000000000000 ) ) ;
#11736 = AXIS2_PLACEMENT_3D ( 'NONE', #9272, #10761, #3709 ) ;
#11737 = CARTESIAN_POINT ( 'NONE',  ( -1.724579595320040015, -1.660794312053859967, 3.098572228637930248 ) ) ;
#11738 = PRODUCT_RELATED_PRODUCT_CATEGORY ( 'part', '', ( #5367 ) ) ;
#11739 = CIRCLE ( 'NONE', #8777, 0.09999999999999982514 ) ;
#11740 = EDGE_CURVE ( 'NONE', #6769, #435, #4557, .T. ) ;
#11741 = CARTESIAN_POINT ( 'NONE',  ( 0.2270348434643680025, -5.304612347394249916, 2.348896311281980065 ) ) ;
#11742 = CARTESIAN_POINT ( 'NONE',  ( -1.132648842710420656, -1.493935417675870791, 7.100045893750492887 ) ) ;
#11743 = EDGE_CURVE ( 'NONE', #14300, #13175, #1924, .T. ) ;
#11744 = FACE_OUTER_BOUND ( 'NONE', #16834, .T. ) ;
#11745 = CARTESIAN_POINT ( 'NONE',  ( 1.000000000000000000, -7.000000000000000000, 5.700000000000000178 ) ) ;
#11746 = EDGE_CURVE ( 'NONE', #11546, #2090, #7456, .T. ) ;
#11747 = CARTESIAN_POINT ( 'NONE',  ( -1.588913656382020756, -5.080331814072260421, 3.399901838171254020 ) ) ;
#11748 = VECTOR ( 'NONE', #11710, 1000.000000000000000 ) ;
#11749 = VECTOR ( 'NONE', #14352, 1000.000000000000000 ) ;
#11750 = CARTESIAN_POINT ( 'NONE',  ( 1.978267656359410154, -0.4023305084745769644, 5.974740860598790171 ) ) ;
#11751 = AXIS2_PLACEMENT_3D ( 'NONE', #12403, #15000, #15190 ) ;
#11752 = CARTESIAN_POINT ( 'NONE',  ( -1.899999999999999911, 2.799999999999999822, 0.6099999999999999867 ) ) ;
#11753 = ORIENTED_EDGE ( 'NONE', *, *, #398, .F. ) ;
#11754 = CARTESIAN_POINT ( 'NONE',  ( 0.9788656693287738353, -5.320452325212859712, 2.556357798777459944 ) ) ;
#11755 = ORIENTED_EDGE ( 'NONE', *, *, #5180, .F. ) ;
#11756 = CARTESIAN_POINT ( 'NONE',  ( -1.899999999999999911, 11.40000000000000036, 7.550000000000000711 ) ) ;
#11757 = VECTOR ( 'NONE', #11402, 1000.000000000000000 ) ;
#11758 = CARTESIAN_POINT ( 'NONE',  ( -0.6914213562373099364, 3.050000000000000266, 2.557842712474620139 ) ) ;
#11759 = VECTOR ( 'NONE', #7521, 1000.000000000000000 ) ;
#11760 = CIRCLE ( 'NONE', #1984, 0.2000000000000000944 ) ;
#11761 = VERTEX_POINT ( 'NONE', #3191 ) ;
#11762 = EDGE_CURVE ( 'NONE', #2304, #16266, #17156, .T. ) ;
#11763 = PLANE ( 'NONE',  #7960 ) ;
#11764 = CARTESIAN_POINT ( 'NONE',  ( -2.159566522375440112, -3.240557039297490061, 5.635424033751089468 ) ) ;
#11765 = VECTOR ( 'NONE', #11153, 1000.000000000000000 ) ;
#11766 = FILL_AREA_STYLE_COLOUR ( '', #5835 ) ;
#11767 = VECTOR ( 'NONE', #12116, 1000.000000000000000 ) ;
#11768 = CARTESIAN_POINT ( 'NONE',  ( 2.351526912647309953, -5.373093220338979847, 4.606040641882800379 ) ) ;
#11769 = CARTESIAN_POINT ( 'NONE',  ( 2.500000000000000000, 2.799999999999999822, 1.600000000000000089 ) ) ;
#11770 = EDGE_CURVE ( 'NONE', #15397, #1059, #7189, .T. ) ;
#11771 = CARTESIAN_POINT ( 'NONE',  ( 0.9170541073686970801, -1.284340823081270067, 6.867431071947180499 ) ) ;
#11772 = CARTESIAN_POINT ( 'NONE',  ( 1.724579595320000047, -3.939205687946140344, 3.098572228637889836 ) ) ;
#11773 = AXIS2_PLACEMENT_3D ( 'NONE', #3358, #11611, #11892 ) ;
#11774 = CARTESIAN_POINT ( 'NONE',  ( 1.966895454505939833, -3.896469987729531681, 5.288408118292026394 ) ) ;
#11775 = AXIS2_PLACEMENT_3D ( 'NONE', #179, #5657, #8616 ) ;
#11776 = CARTESIAN_POINT ( 'NONE',  ( 0.1365430262726380628, -0.1468220338983061424, 6.748423079423377047 ) ) ;
#11777 = FACE_OUTER_BOUND ( 'NONE', #5431, .T. ) ;
#11778 = CARTESIAN_POINT ( 'NONE',  ( -1.289999999999999813, 7.900000000000003908, 3.000000000000002220 ) ) ;
#11779 = ORIENTED_EDGE ( 'NONE', *, *, #3281, .T. ) ;
#11780 = VECTOR ( 'NONE', #6884, 1000.000000000000000 ) ;
#11781 = CARTESIAN_POINT ( 'NONE',  ( 1.647941990407678636, -0.3444915254237289615, 3.475676388127089123 ) ) ;
#11782 = CARTESIAN_POINT ( 'NONE',  ( -1.507201387235980183, -3.124115597856050197, 6.507509243627219497 ) ) ;
#11783 = EDGE_LOOP ( 'NONE', ( #2384, #7443, #2432, #19 ) ) ;
#11784 = ORIENTED_EDGE ( 'NONE', *, *, #90, .F. ) ;
#11785 = CYLINDRICAL_SURFACE ( 'NONE', #15071, 0.1499999999999999667 ) ;
#11786 = ORIENTED_EDGE ( 'NONE', *, *, #14794, .T. ) ;
#11787 = CARTESIAN_POINT ( 'NONE',  ( 2.316639661709690046, -3.780028546288089153, 4.285359956977720763 ) ) ;
#11788 = VECTOR ( 'NONE', #1902, 1000.000000000000000 ) ;
#11789 = CONTEXT_DEPENDENT_SHAPE_REPRESENTATION ( #1779, #13779 ) ;
#11790 = CARTESIAN_POINT ( 'NONE',  ( 2.578017356471871135, -5.086440677966105994, 5.329826563567761077 ) ) ;
#11791 = CIRCLE ( 'NONE', #8252, 0.3999999999999999667 ) ;
#11792 = AXIS2_PLACEMENT_3D ( 'NONE', #12338, #7796, #6589 ) ;
#11793 = DIRECTION ( 'NONE',  ( -0.7071067811865470176, 0.7071067811865480168, 0.000000000000000000 ) ) ;
#11794 = CARTESIAN_POINT ( 'NONE',  ( -1.713314936023349944, -0.5610169491525430763, 3.089913064446579760 ) ) ;
#11795 = ORIENTED_EDGE ( 'NONE', *, *, #11451, .F. ) ;
#11796 = EDGE_CURVE ( 'NONE', #2787, #13022, #10397, .T. ) ;
#11797 = CARTESIAN_POINT ( 'NONE',  ( 0.1749999999999999889, 9.299999999999998934, 0.4000000000000000222 ) ) ;
#11798 = CYLINDRICAL_SURFACE ( 'NONE', #2882, 0.7000000000000000666 ) ;
#11799 = CARTESIAN_POINT ( 'NONE',  ( 1.366362128262241571, -3.915917399657852904, 3.167695729602394206 ) ) ;
#11800 = CARTESIAN_POINT ( 'NONE',  ( -1.851400890972779045, -0.4868644067796619179, 6.601359968904141340 ) ) ;
#11801 = ORIENTED_EDGE ( 'NONE', *, *, #1780, .T. ) ;
#11802 = AXIS2_PLACEMENT_3D ( 'NONE', #3294, #13189, #9496 ) ;
#11803 = DIRECTION ( 'NONE',  ( 1.000000000000000000, 0.000000000000000000, 0.000000000000000000 ) ) ;
#11804 = ORIENTED_EDGE ( 'NONE', *, *, #16295, .F. ) ;
#11805 = CARTESIAN_POINT ( 'NONE',  ( 0.008535039157541330149, -0.3147268565821629838, 2.281464080633810010 ) ) ;
#11806 = LINE ( 'NONE', #14943, #3207 ) ;
#11807 = CARTESIAN_POINT ( 'NONE',  ( -1.661700935788390288, -0.2625000000000000111, 3.038299064211610112 ) ) ;
#11808 = CARTESIAN_POINT ( 'NONE',  ( 0.6919952253610313075, -4.451548030288480895, 7.262080463427998289 ) ) ;
#11809 = ORIENTED_EDGE ( 'NONE', *, *, #15612, .F. ) ;
#11810 = AXIS2_PLACEMENT_3D ( 'NONE', #8450, #15766, #11502 ) ;
#11811 = CARTESIAN_POINT ( 'NONE',  ( 1.669205944673859854, -2.452596113855660231, 6.359065158982410537 ) ) ;
#11812 = LINE ( 'NONE', #15888, #4938 ) ;
#11813 = DIRECTION ( 'NONE',  ( 0.2721173643531200059, 0.9622640697945191723, 0.000000000000000000 ) ) ;
#11814 = CARTESIAN_POINT ( 'NONE',  ( 1.727468145286579659, -3.966334852594401994, 5.809394271505055052 ) ) ;
#11815 = CYLINDRICAL_SURFACE ( 'NONE', #13534, 0.5000000000000000000 ) ;
#11816 = CARTESIAN_POINT ( 'NONE',  ( 1.899999999999999911, 3.500000000000000000, 0.6099999999999999867 ) ) ;
#11817 = CARTESIAN_POINT ( 'NONE',  ( 1.417606053559480328, -0.8922807985403484743, 6.185023541745921172 ) ) ;
#11818 = ORIENTED_EDGE ( 'NONE', *, *, #340, .F. ) ;
#11819 = PLANE ( 'NONE',  #817 ) ;
#11820 = FACE_OUTER_BOUND ( 'NONE', #12449, .T. ) ;
#11821 = CARTESIAN_POINT ( 'NONE',  ( -2.107551805806941125, -1.311469987729540376, 6.312866726931216199 ) ) ;
#11822 = ORIENTED_EDGE ( 'NONE', *, *, #12842, .F. ) ;
#11823 = CIRCLE ( 'NONE', #3837, 1.100000000000000311 ) ;
#11824 = CARTESIAN_POINT ( 'NONE',  ( -2.135041058613629694, -4.800872354612799597, 5.690123914223820023 ) ) ;
#11825 = DIRECTION ( 'NONE',  ( 8.326672684688670109E-16, 0.000000000000000000, 1.000000000000000000 ) ) ;
#11826 = CARTESIAN_POINT ( 'NONE',  ( 2.500000000000000000, 8.500000000000000000, 0.6099999999999999867 ) ) ;
#11827 = CARTESIAN_POINT ( 'NONE',  ( -0.5889081234606770021, -5.162076271186439413, 6.978529000034869867 ) ) ;
#11828 = VERTEX_POINT ( 'NONE', #4398 ) ;
#11829 = ORIENTED_EDGE ( 'NONE', *, *, #3124, .T. ) ;
#11830 = CARTESIAN_POINT ( 'NONE',  ( -1.750000000000000000, 0.5999999999999999778, 7.550000000000000711 ) ) ;
#11831 =( NAMED_UNIT ( * ) PLANE_ANGLE_UNIT ( ) SI_UNIT ( $, .RADIAN. ) );
#11832 = CARTESIAN_POINT ( 'NONE',  ( -1.408343819019460219E-16, 2.299999999999999822, 5.100000000000000533 ) ) ;
#11833 = ORIENTED_EDGE ( 'NONE', *, *, #5650, .T. ) ;
#11834 = CARTESIAN_POINT ( 'NONE',  ( -4.163799117100999573E-16, 6.450000000000000178, 3.949485927250209908E-16 ) ) ;
#11835 = CARTESIAN_POINT ( 'NONE',  ( 2.212163452524050111, -2.704926408666860738, 6.166099093621837390 ) ) ;
#11836 = CARTESIAN_POINT ( 'NONE',  ( 0.5110358699406184479, -0.3612150962701983770, 2.697283651280069527 ) ) ;
#11837 = CARTESIAN_POINT ( 'NONE',  ( -0.009452110982655708218, -0.5998079552954630467, 2.350000000000000089 ) ) ;
#11838 = CIRCLE ( 'NONE', #1499, 0.04999999999999969746 ) ;
#11839 = CARTESIAN_POINT ( 'NONE',  ( -2.075124426334559846, -2.918361879621429900, 5.810227140144559321 ) ) ;
#11840 = CARTESIAN_POINT ( 'NONE',  ( -0.3042893218813459977, 3.050000000000000266, 2.029289321881350361 ) ) ;
#11841 = CARTESIAN_POINT ( 'NONE',  ( 2.650521604678268694, -1.004881363621820567, 4.833599835830299618 ) ) ;
#11842 = PLANE ( 'NONE',  #3711 ) ;
#11843 = EDGE_CURVE ( 'NONE', #16255, #2694, #16060, .T. ) ;
#11844 = CARTESIAN_POINT ( 'NONE',  ( 0.7983658734558030101, -0.4334745762711870176, 6.913847129767330735 ) ) ;
#11845 = LINE ( 'NONE', #11651, #1783 ) ;
#11846 = VERTEX_POINT ( 'NONE', #14571 ) ;
#11847 = DIRECTION ( 'NONE',  ( 1.000000000000000000, 1.734723475976809806E-16, 1.110223024625159992E-16 ) ) ;
#11848 = ORIENTED_EDGE ( 'NONE', *, *, #6133, .F. ) ;
#11849 = PLANE ( 'NONE',  #12623 ) ;
#11850 = AXIS2_PLACEMENT_3D ( 'NONE', #1996, #9415, #5244 ) ;
#11851 = DIRECTION ( 'NONE',  ( 1.224646799147349263E-16, 0.000000000000000000, 1.000000000000000000 ) ) ;
#11852 = EDGE_CURVE ( 'NONE', #12486, #11896, #11699, .T. ) ;
#11853 = ORIENTED_EDGE ( 'NONE', *, *, #5521, .F. ) ;
#11854 = EDGE_CURVE ( 'NONE', #17047, #6319, #14391, .T. ) ;
#11855 = EDGE_CURVE ( 'NONE', #7200, #16687, #1885, .T. ) ;
#11856 = DIRECTION ( 'NONE',  ( -0.7071067811865470176, 0.7071067811865480168, 0.000000000000000000 ) ) ;
#11857 = CARTESIAN_POINT ( 'NONE',  ( 1.764807890102179977, -2.378890372630820149, 3.143016121304719857 ) ) ;
#11858 = CARTESIAN_POINT ( 'NONE',  ( 3.367778697655222491E-17, 2.049999999999999822, 7.700000000000000178 ) ) ;
#11859 = CARTESIAN_POINT ( 'NONE',  ( 1.677844243193131746, -0.4963825586767564024, 3.040248005478333848 ) ) ;
#11860 = CARTESIAN_POINT ( 'NONE',  ( -1.661700935788390066, -0.5625000000000000000, 3.038299064211610112 ) ) ;
#11861 = CARTESIAN_POINT ( 'NONE',  ( 1.652654650382400003, -0.7952867690272209522, 3.029252778805620050 ) ) ;
#11862 = VECTOR ( 'NONE', #12057, 1000.000000000000000 ) ;
#11863 = CARTESIAN_POINT ( 'NONE',  ( 2.262450597846779932, -4.195376859117310175, 5.348122657979680561 ) ) ;
#11864 = CARTESIAN_POINT ( 'NONE',  ( 1.872456193198871022, -1.098034516774970770, 5.541908336565965598 ) ) ;
#11865 = DIRECTION ( 'NONE',  ( -4.485749594445070317E-16, 0.000000000000000000, -1.000000000000000000 ) ) ;
#11866 = LINE ( 'NONE', #4806, #11218 ) ;
#11867 = ORIENTED_EDGE ( 'NONE', *, *, #6178, .F. ) ;
#11868 = EDGE_CURVE ( 'NONE', #16856, #16401, #8657, .T. ) ;
#11869 = CARTESIAN_POINT ( 'NONE',  ( -1.494593880360799432, -0.2610169491525428653, 3.295456077495951153 ) ) ;
#11870 = CARTESIAN_POINT ( 'NONE',  ( 2.343457872958619959, -4.148800282540729967, 4.916681529328559286 ) ) ;
#11871 = EDGE_LOOP ( 'NONE', ( #15536, #7016, #12050, #12828 ) ) ;
#11872 = ORIENTED_EDGE ( 'NONE', *, *, #13100, .F. ) ;
#11873 = LINE ( 'NONE', #8986, #12966 ) ;
#11874 = EDGE_CURVE ( 'NONE', #1792, #6773, #4835, .T. ) ;
#11875 = EDGE_LOOP ( 'NONE', ( #314, #8484, #1283, #8981 ) ) ;
#11876 = CARTESIAN_POINT ( 'NONE',  ( 1.850000000000000089, -6.000000000000000000, 6.899999999999999467 ) ) ;
#11877 = EDGE_CURVE ( 'NONE', #16167, #14474, #14850, .T. ) ;
#11878 = CARTESIAN_POINT ( 'NONE',  ( -2.653602652190420574, -5.224364406779660186, 4.735326402787099376 ) ) ;
#11879 = CARTESIAN_POINT ( 'NONE',  ( 6.429395695523600208E-16, 3.500000000000000000, 5.100000000000000533 ) ) ;
#11880 = CARTESIAN_POINT ( 'NONE',  ( 0.7983658734558030101, -0.4334745762711870176, 6.913847129767330735 ) ) ;
#11881 = EDGE_LOOP ( 'NONE', ( #17954, #1904, #7112, #3808 ) ) ;
#11882 = CARTESIAN_POINT ( 'NONE',  ( 0.03000000000000110217, 11.40000000000000036, 7.649999999999999467 ) ) ;
#11883 = CARTESIAN_POINT ( 'NONE',  ( 9.797174393178831574E-16, -8.000000000000000000, -4.898587196589410857E-16 ) ) ;
#11884 = CARTESIAN_POINT ( 'NONE',  ( -0.6050872056802790722, -3.659746228486683073, 2.738171435586149727 ) ) ;
#11885 = CARTESIAN_POINT ( 'NONE',  ( -2.578017356471871135, -0.5135593220338985354, 5.329826563567776176 ) ) ;
#11886 = ORIENTED_EDGE ( 'NONE', *, *, #11051, .T. ) ;
#11887 = LINE ( 'NONE', #6397, #4364 ) ;
#11888 = ORIENTED_EDGE ( 'NONE', *, *, #16146, .T. ) ;
#11889 = CARTESIAN_POINT ( 'NONE',  ( 1.800129581279440893, -0.03559322033898339871, 2.750028594811110061 ) ) ;
#11890 = ORIENTED_EDGE ( 'NONE', *, *, #359, .F. ) ;
#11891 = DIRECTION ( 'NONE',  ( 1.000000000000000000, 0.000000000000000000, 0.000000000000000000 ) ) ;
#11892 = DIRECTION ( 'NONE',  ( -0.9622640697945192834, -0.2721173643531198949, 0.000000000000000000 ) ) ;
#11893 = EDGE_CURVE ( 'NONE', #1463, #16167, #768, .T. ) ;
#11894 = CARTESIAN_POINT ( 'NONE',  ( 0.7983658734558031211, -0.1334745762711870287, 6.913847129767330735 ) ) ;
#11895 = CARTESIAN_POINT ( 'NONE',  ( -0.04351999560413650353, -4.521412895153344103, 7.353529668759054339 ) ) ;
#11896 = VERTEX_POINT ( 'NONE', #10681 ) ;
#11897 = CARTESIAN_POINT ( 'NONE',  ( -0.3413183941262150078, -2.685478996738539958, 7.028571974690709823 ) ) ;
#11898 = DIRECTION ( 'NONE',  ( -1.000000000000000000, 0.000000000000000000, 0.000000000000000000 ) ) ;
#11899 = LINE ( 'NONE', #14253, #6956 ) ;
#11900 = CARTESIAN_POINT ( 'NONE',  ( -1.854389246811851022, -3.151244762504313179, 3.819010576716904026 ) ) ;
#11901 = LINE ( 'NONE', #7819, #5838 ) ;
#11902 = CARTESIAN_POINT ( 'NONE',  ( -0.5381211601353440566, -1.148451969711520082, 6.681243917250651698 ) ) ;
#11903 = ORIENTED_EDGE ( 'NONE', *, *, #15041, .T. ) ;
#11904 = CARTESIAN_POINT ( 'NONE',  ( 1.307725206348619995, -0.7471169921413569615, 2.732408283416570161 ) ) ;
#11905 = VECTOR ( 'NONE', #5786, 1000.000000000000000 ) ;
#11906 = VERTEX_POINT ( 'NONE', #14942 ) ;
#11907 = CARTESIAN_POINT ( 'NONE',  ( 2.500000000000000000, 10.00000000000000000, 1.600000000000000089 ) ) ;
#11908 = FACE_OUTER_BOUND ( 'NONE', #8465, .T. ) ;
#11909 = CARTESIAN_POINT ( 'NONE',  ( 8.549934884138839976E-16, 6.262741699796950279, 5.100000000000000533 ) ) ;
#11910 = CARTESIAN_POINT ( 'NONE',  ( -0.8570167067220350043, -5.282203389830510076, 2.508190348879359988 ) ) ;
#11911 = VERTEX_POINT ( 'NONE', #13555 ) ;
#11912 = EDGE_CURVE ( 'NONE', #12628, #8096, #16089, .T. ) ;
#11913 = ORIENTED_EDGE ( 'NONE', *, *, #4590, .T. ) ;
#11914 = FACE_OUTER_BOUND ( 'NONE', #11705, .T. ) ;
#11915 = CYLINDRICAL_SURFACE ( 'NONE', #10572, 0.2000000000000000111 ) ;
#11916 = FACE_OUTER_BOUND ( 'NONE', #4790, .T. ) ;
#11917 = ORIENTED_EDGE ( 'NONE', *, *, #1809, .F. ) ;
#11918 = DIRECTION ( 'NONE',  ( 0.000000000000000000, 0.000000000000000000, 1.000000000000000000 ) ) ;
#11919 = CARTESIAN_POINT ( 'NONE',  ( 2.619177996481910853, -2.518620102360551893, 4.272191262657148769 ) ) ;
#11920 = ADVANCED_FACE ( 'NONE', ( #16738 ), #17095, .T. ) ;
#11921 = DIRECTION ( 'NONE',  ( 1.073215590470990073E-14, 1.000000000000000000, 0.000000000000000000 ) ) ;
#11922 = CIRCLE ( 'NONE', #677, 0.7211102550927980248 ) ;
#11923 = FACE_OUTER_BOUND ( 'NONE', #12665, .T. ) ;
#11924 = CARTESIAN_POINT ( 'NONE',  ( 2.340959815966380031, -3.849893411152960354, 4.942183458383420103 ) ) ;
#11926 = VERTEX_POINT ( 'NONE', #5453 ) ;
#11925 = CARTESIAN_POINT ( 'NONE',  ( 2.174104834890520976, -1.144611093351550091, 6.221966445066246187 ) ) ;
#11927 = CARTESIAN_POINT ( 'NONE',  ( 2.500000000000000000, 7.299999999999999822, 0.6099999999999999867 ) ) ;
#11928 = AXIS2_PLACEMENT_3D ( 'NONE', #15205, #9349, #17948 ) ;
#11929 = CARTESIAN_POINT ( 'NONE',  ( 1.399999999999999911, 6.400000000000000355, 7.700000000000000178 ) ) ;
#11930 = FACE_OUTER_BOUND ( 'NONE', #1275, .T. ) ;
#11931 = CARTESIAN_POINT ( 'NONE',  ( 2.043014502273419186, -5.341949152542365908, 3.006203457898239062 ) ) ;
#11932 = ORIENTED_EDGE ( 'NONE', *, *, #15225, .T. ) ;
#11933 = VECTOR ( 'NONE', #17448, 1000.000000000000000 ) ;
#11934 = LINE ( 'NONE', #6191, #12543 ) ;
#11935 = EDGE_LOOP ( 'NONE', ( #15153, #10641, #11422, #15211 ) ) ;
#11936 = CARTESIAN_POINT ( 'NONE',  ( -1.875000000000000000, 12.00000000000000000, 7.700000000000000178 ) ) ;
#11937 = ORIENTED_EDGE ( 'NONE', *, *, #2055, .T. ) ;
#11938 = EDGE_CURVE ( 'NONE', #15780, #15692, #286, .T. ) ;
#11939 = CARTESIAN_POINT ( 'NONE',  ( -1.236334101859210000, -2.029566048306499670, 2.697445712080720259 ) ) ;
#11940 = PLANE ( 'NONE',  #6142 ) ;
#11941 = CARTESIAN_POINT ( 'NONE',  ( 3.673940397442067510E-17, 2.600000000000000089, 7.750000000000000000 ) ) ;
#11942 = DIRECTION ( 'NONE',  ( 0.000000000000000000, 6.123233995736769734E-17, -1.000000000000000000 ) ) ;
#11943 = CARTESIAN_POINT ( 'NONE',  ( -2.340959815966380031, -1.750106588847040179, 4.942183458383479611 ) ) ;
#11944 = CARTESIAN_POINT ( 'NONE',  ( 0.6096110657044089276, -3.799475958216410376, 2.426869991387509806 ) ) ;
#11945 = CARTESIAN_POINT ( 'NONE',  ( 1.683529720875211799, -1.144611093351550091, 5.875001924065625936 ) ) ;
#11946 = DIRECTION ( 'NONE',  ( 2.220446049250309876E-16, 1.000000000000000000, -1.192513461937156062E-31 ) ) ;
#11947 = ADVANCED_FACE ( 'NONE', ( #12769 ), #11461, .T. ) ;
#11948 = CARTESIAN_POINT ( 'NONE',  ( -1.449568901432419343, -0.5625000000000005551, 3.250431098567584165 ) ) ;
#11949 = DIRECTION ( 'NONE',  ( -3.700743415417195042E-15, -3.289549702593060375E-15, 1.000000000000000000 ) ) ;
#11950 = EDGE_LOOP ( 'NONE', ( #13004, #18123, #9230, #756 ) ) ;
#11951 = CARTESIAN_POINT ( 'NONE',  ( -1.399999999999999911, 6.400000000000000355, 8.300000000000000711 ) ) ;
#11952 = CARTESIAN_POINT ( 'NONE',  ( -0.2453710345350140487, -0.1557203389830511819, 6.738252723719333481 ) ) ;
#11953 = CARTESIAN_POINT ( 'NONE',  ( 2.262450597846779932, -4.195376859117310175, 5.348122657979680561 ) ) ;
#11954 = ORIENTED_EDGE ( 'NONE', *, *, #4151, .T. ) ;
#11955 = ORIENTED_EDGE ( 'NONE', *, *, #12876, .F. ) ;
#11956 = CARTESIAN_POINT ( 'NONE',  ( 0.3750000000000000000, 6.450000000000000178, 2.100000000000000089 ) ) ;
#11957 = ORIENTED_EDGE ( 'NONE', *, *, #7660, .F. ) ;
#11958 = CARTESIAN_POINT ( 'NONE',  ( -1.652654650382402668, -4.804713230972782689, 3.029252778805632484 ) ) ;
#11959 = ITEM_DEFINED_TRANSFORMATION ( 'NONE', 'NONE', #10599,  #17681 ) ;
#11960 = CARTESIAN_POINT ( 'NONE',  ( -0.1565249325564300187, -5.153177966101689655, 7.048192310558509810 ) ) ;
#11961 = CARTESIAN_POINT ( 'NONE',  ( -11.62823001646930088, 1.318530427328540049E-14, 0.5999999999999559019 ) ) ;
#11962 = CARTESIAN_POINT ( 'NONE',  ( 1.978267656359410154, -0.4023305084745769644, 5.974740860598790171 ) ) ;
#11963 = ORIENTED_EDGE ( 'NONE', *, *, #15724, .F. ) ;
#11964 = EDGE_CURVE ( 'NONE', #305, #1875, #15652, .T. ) ;
#11965 = CARTESIAN_POINT ( 'NONE',  ( -0.2220816246931631155, -4.544701183441625325, 6.740975647723836950 ) ) ;
#11966 = EDGE_CURVE ( 'NONE', #5781, #9046, #4052, .T. ) ;
#11967 = ADVANCED_FACE ( 'NONE', ( #12575 ), #4233, .F. ) ;
#11968 = CARTESIAN_POINT ( 'NONE',  ( 1.255262969126039558E-16, -2.775557561562890858E-16, 2.050000000000001155 ) ) ;
#11969 = ORIENTED_EDGE ( 'NONE', *, *, #9049, .T. ) ;
#11970 = EDGE_CURVE ( 'NONE', #7523, #4252, #15734, .T. ) ;
#11971 = EDGE_CURVE ( 'NONE', #12787, #17179, #15374, .T. ) ;
#11972 = VECTOR ( 'NONE', #9098, 1000.000000000000000 ) ;
#11973 = ORIENTED_EDGE ( 'NONE', *, *, #5115, .F. ) ;
#11974 = CARTESIAN_POINT ( 'NONE',  ( 2.601107615185130673, -0.3845338983050847759, 5.226397344856369642 ) ) ;
#11975 = EDGE_CURVE ( 'NONE', #1650, #3610, #4322, .T. ) ;
#11976 = ORIENTED_EDGE ( 'NONE', *, *, #199, .F. ) ;
#11977 = CARTESIAN_POINT ( 'NONE',  ( -1.057242234132100167, -5.577754237288139905, 2.597442975781530272 ) ) ;
#11978 = CARTESIAN_POINT ( 'NONE',  ( -1.026235786675429473, -1.195028546288090077, 6.817920158464569447 ) ) ;
#11979 = CARTESIAN_POINT ( 'NONE',  ( -0.7101077586918816964, -0.2831443699174400752, 2.770804889310179764 ) ) ;
#11980 = CARTESIAN_POINT ( 'NONE',  ( 2.105672170043351166, -3.962493976234419790, 3.084680091961101045 ) ) ;
#11981 = ORIENTED_EDGE ( 'NONE', *, *, #10319, .F. ) ;
#11982 = CARTESIAN_POINT ( 'NONE',  ( 0.009452110982653640428, -5.000192044704539818, 2.350000000000000089 ) ) ;
#11983 = CARTESIAN_POINT ( 'NONE',  ( 1.881914957835459923, -3.663587104846649734, 3.286797332666310023 ) ) ;
#11984 = CARTESIAN_POINT ( 'NONE',  ( -1.670747221194377685, -5.103620102360557631, 3.047345349617607724 ) ) ;
#11985 = LINE ( 'NONE', #4939, #2154 ) ;
#11986 = CARTESIAN_POINT ( 'NONE',  ( 0.1352600594606461204, -4.199217735477280833, 6.748562071049542865 ) ) ;
#11988 = EDGE_CURVE ( 'NONE', #11460, #14967, #10081, .T. ) ;
#11987 = CARTESIAN_POINT ( 'NONE',  ( -1.899999999999999911, 2.000000000000000000, 0.5999999999999999778 ) ) ;
#11989 = DIRECTION ( 'NONE',  ( 1.224646799147350002E-16, -1.000000000000000000, -6.123233995736769734E-17 ) ) ;
#11990 = CARTESIAN_POINT ( 'NONE',  ( -1.366362128262280429, -1.684082600342149627, 3.167695729602423516 ) ) ;
#11991 = VERTEX_POINT ( 'NONE', #7209 ) ;
#11992 = LINE ( 'NONE', #17712, #15043 ) ;
#11993 = VECTOR ( 'NONE', #12711, 1000.000000000000000 ) ;
#11994 = PLANE ( 'NONE',  #6763 ) ;
#11995 = EDGE_LOOP ( 'NONE', ( #3178, #6675, #1414, #15731, #13440, #1185, #5639, #8626, #4168, #7563, #14974, #485, #2446, #9819, #3804, #7476, #6165, #2528, #17022, #1554, #338, #14443, #5725, #5661, #7788, #3650 ) ) ;
#11996 = PLANE ( 'NONE',  #2325 ) ;
#11997 = LINE ( 'NONE', #18241, #4781 ) ;
#11998 = DIRECTION ( 'NONE',  ( 0.000000000000000000, 2.960594732333760372E-15, -1.000000000000000000 ) ) ;
#11999 = CARTESIAN_POINT ( 'NONE',  ( -1.057242234132100167, -5.277754237288139194, 2.597442975781530272 ) ) ;
#12000 = EDGE_LOOP ( 'NONE', ( #575, #12834, #9761, #14902 ) ) ;
#12001 = ORIENTED_EDGE ( 'NONE', *, *, #13870, .T. ) ;
#12002 = CARTESIAN_POINT ( 'NONE',  ( -1.889999999999999902, 4.700000000000000178, 0.5999999999999999778 ) ) ;
#12003 = DIRECTION ( 'NONE',  ( -4.898587196589410857E-16, -1.000000000000000000, 0.000000000000000000 ) ) ;
#12004 = DIRECTION ( 'NONE',  ( -1.000000000000000000, 2.220446049250309876E-16, 0.000000000000000000 ) ) ;
#12005 = VERTEX_POINT ( 'NONE', #3039 ) ;
#12006 = CARTESIAN_POINT ( 'NONE',  ( -2.022304719220918479, -5.533262711864405325, 4.346496488058700258 ) ) ;
#12007 = CARTESIAN_POINT ( 'NONE',  ( 2.197904923864649529, -2.406019537279079579, 6.187389538303071923 ) ) ;
#12008 = CARTESIAN_POINT ( 'NONE',  ( -1.503451935564901643, -3.100827309567759205, 6.886949009567437052 ) ) ;
#12009 = AXIS2_PLACEMENT_3D ( 'NONE', #17711, #3740, #8780 ) ;
#12010 = CARTESIAN_POINT ( 'NONE',  ( -1.899999999999999911, 11.15000000000000036, 1.600000000000000089 ) ) ;
#12011 = CARTESIAN_POINT ( 'NONE',  ( -2.500000000000000000, 10.00000000000000000, 1.600000000000000089 ) ) ;
#12012 = CARTESIAN_POINT ( 'NONE',  ( 1.417709711196429856, -3.593722239981790079, 2.821478011237759986 ) ) ;
#12014 = ADVANCED_FACE ( 'NONE', ( #6928 ), #5727, .T. ) ;
#12013 = DIRECTION ( 'NONE',  ( -2.220446049250309876E-16, 0.000000000000000000, -1.000000000000000000 ) ) ;
#12015 = DIRECTION ( 'NONE',  ( 0.000000000000000000, 1.000000000000000000, 0.000000000000000000 ) ) ;
#12017 = ORIENTED_EDGE ( 'NONE', *, *, #5976, .F. ) ;
#12016 = CARTESIAN_POINT ( 'NONE',  ( -1.176011442874419943, -2.052854336594789331, 2.320901267448050476 ) ) ;
#12018 = CARTESIAN_POINT ( 'NONE',  ( -1.000000000000000000, 6.799999999999999822, 8.300000000000000711 ) ) ;
#12019 = CARTESIAN_POINT ( 'NONE',  ( -1.899999999999999911, 0.5999999999999999778, 1.600000000000000089 ) ) ;
#12020 = CARTESIAN_POINT ( 'NONE',  ( 0.1749999999999999889, 7.700000000000000178, 0.4000000000000000222 ) ) ;
#12021 = CARTESIAN_POINT ( 'NONE',  ( 0.01716182025089369942, -2.169295778036230082, 2.346608583467340026 ) ) ;
#12022 = CARTESIAN_POINT ( 'NONE',  ( 0.009452039534070141164, -0.3001931771041043140, 2.350000000173209092 ) ) ;
#12023 = CARTESIAN_POINT ( 'NONE',  ( -0.6493550500446439999, -5.586652542372879005, 2.437955526623099889 ) ) ;
#12024 = ORIENTED_EDGE ( 'NONE', *, *, #207, .T. ) ;
#12025 = VECTOR ( 'NONE', #10673, 1000.000000000000000 ) ;
#12026 = CIRCLE ( 'NONE', #3723, 0.5999999999999998668 ) ;
#12027 = LINE ( 'NONE', #17384, #14606 ) ;
#12028 = EDGE_LOOP ( 'NONE', ( #8771, #4499, #10965, #7633, #17686, #14379, #9562, #17359 ) ) ;
#12029 = FACE_OUTER_BOUND ( 'NONE', #17427, .T. ) ;
#12030 = DIRECTION ( 'NONE',  ( -1.000000000000000000, 0.000000000000000000, 0.000000000000000000 ) ) ;
#12031 = EDGE_LOOP ( 'NONE', ( #3559, #16193, #12704, #1324 ) ) ;
#12032 = AXIS2_PLACEMENT_3D ( 'NONE', #3103, #7006, #15717 ) ;
#12033 = ORIENTED_EDGE ( 'NONE', *, *, #13128, .F. ) ;
#12034 = CARTESIAN_POINT ( 'NONE',  ( -0.9485663501270049647, -3.054250732991179440, 6.853826262002260528 ) ) ;
#12035 = CARTESIAN_POINT ( 'NONE',  ( 0.2812789908084389889, -5.444279661016950378, 7.036533610117280624 ) ) ;
#12036 = FACE_OUTER_BOUND ( 'NONE', #15482, .T. ) ;
#12037 = VECTOR ( 'NONE', #14988, 1000.000000000000000 ) ;
#12038 = CARTESIAN_POINT ( 'NONE',  ( -2.005512128484160161, -1.913124606865060029, 3.468469736471389897 ) ) ;
#12039 = VECTOR ( 'NONE', #5933, 1000.000000000000000 ) ;
#12040 = CARTESIAN_POINT ( 'NONE',  ( 0.3949552299394610277, -3.776187669928119828, 2.379923265530350385 ) ) ;
#12041 = CARTESIAN_POINT ( 'NONE',  ( -1.903446074666951260, -1.680241723982170754, 5.469282057156605426 ) ) ;
#12042 = PLANE ( 'NONE',  #12947 ) ;
#12043 = VECTOR ( 'NONE', #15037, 1000.000000000000000 ) ;
#12044 = VECTOR ( 'NONE', #14639, 1000.000000000000000 ) ;
#12045 = DIRECTION ( 'NONE',  ( 0.000000000000000000, 0.000000000000000000, -1.000000000000000000 ) ) ;
#12046 = ORIENTED_EDGE ( 'NONE', *, *, #18056, .T. ) ;
#12047 = CARTESIAN_POINT ( 'NONE',  ( 1.641313093088730080, -5.335726896972119881, 3.058686906911260106 ) ) ;
#12048 = CARTESIAN_POINT ( 'NONE',  ( 0.5999999999999999778, 0.5999999999999999778, 7.599999999999999645 ) ) ;
#12049 = CARTESIAN_POINT ( 'NONE',  ( 0.6096110657044089276, -3.799475958216410376, 2.426869991387509806 ) ) ;
#12050 = ORIENTED_EDGE ( 'NONE', *, *, #10606, .F. ) ;
#12051 = ORIENTED_EDGE ( 'NONE', *, *, #11410, .F. ) ;
#12052 = B_SPLINE_CURVE_WITH_KNOTS ( 'NONE', 3,
 ( #11180, #6836, #2950, #6742, #12567, #3955, #18013, #16727, #5444, #8321, #9979, #7124, #15266, #14044, #12480 ),
 .UNSPECIFIED., .F., .F.,
 ( 4, 1, 1, 1, 1, 1, 1, 1, 1, 1, 1, 1, 4 ),
 ( 0.000000000000000000, 0.04238993203358450146, 0.08487769703118749898, 0.1274691104749350046, 0.1700369147468580033, 0.2126104510726569974, 0.2551841450615619511, 0.2977574123560440267, 0.3403308656858579639, 0.3829042603267339695, 0.4254776701663789962, 0.4680510765563200004, 0.4999998211434326656 ),
 .UNSPECIFIED. ) ;
#12053 = CARTESIAN_POINT ( 'NONE',  ( -0.4000000000000000222, 2.399999999999999911, 5.100000000000000533 ) ) ;
#12054 = VECTOR ( 'NONE', #9397, 1000.000000000000000 ) ;
#12055 = ORIENTED_EDGE ( 'NONE', *, *, #12439, .F. ) ;
#12056 = VECTOR ( 'NONE', #15987, 1000.000000000000000 ) ;
#12057 = DIRECTION ( 'NONE',  ( -1.000000000000000000, 0.000000000000000000, 0.000000000000000000 ) ) ;
#12058 = CARTESIAN_POINT ( 'NONE',  ( -1.549742865090599997, -5.184322033898309812, 6.471102547561460305 ) ) ;
#12059 = DIRECTION ( 'NONE',  ( 1.000000000000000000, 1.233581138472399909E-16, 2.220446049250309876E-16 ) ) ;
#12060 = CARTESIAN_POINT ( 'NONE',  ( 1.750000000000000000, 0.5999999999999999778, 7.550000000000000711 ) ) ;
#12061 = CIRCLE ( 'NONE', #4073, 0.04999999999999969746 ) ;
#12062 = CARTESIAN_POINT ( 'NONE',  ( 1.399999999999999911, -5.500000000000000000, 6.100000000000000533 ) ) ;
#12063 = CARTESIAN_POINT ( 'NONE',  ( -0.7778405029480311983, -4.614566048306495638, 6.599964735094220991 ) ) ;
#12064 = CARTESIAN_POINT ( 'NONE',  ( -2.416676968769249090, -0.5046610169491535514, 5.796598111919839980 ) ) ;
#12065 = VECTOR ( 'NONE', #6439, 1000.000000000000000 ) ;
#12066 = ORIENTED_EDGE ( 'NONE', *, *, #398, .T. ) ;
#12067 = CARTESIAN_POINT ( 'NONE',  ( 2.011500846714319835, -0.3489406779661020086, 3.478373409938460448 ) ) ;
#12068 = CARTESIAN_POINT ( 'NONE',  ( 2.011500846714319835, -0.04894067796610199889, 3.478373409938460448 ) ) ;
#12069 = ORIENTED_EDGE ( 'NONE', *, *, #11855, .T. ) ;
#12070 = VECTOR ( 'NONE', #1277, 1000.000000000000000 ) ;
#12071 = VECTOR ( 'NONE', #6315, 1000.000000000000000 ) ;
#12072 = CARTESIAN_POINT ( 'NONE',  ( -1.549742865090599997, -5.484322033898309634, 6.471102547561460305 ) ) ;
#12073 = EDGE_CURVE ( 'NONE', #14013, #15707, #8950, .T. ) ;
#12074 = CARTESIAN_POINT ( 'NONE',  ( -1.869848057046539669, -1.311469987729539710, 6.129130480762059463 ) ) ;
#12075 = CARTESIAN_POINT ( 'NONE',  ( 2.234315482767910144, -5.359745762711869865, 3.960850823455320580 ) ) ;
#12076 = EDGE_CURVE ( 'NONE', #15692, #3882, #14809, .T. ) ;
#12077 = CARTESIAN_POINT ( 'NONE',  ( -0.9279264017968105183, -1.171740257999810852, 7.186376135231811624 ) ) ;
#12078 = ORIENTED_EDGE ( 'NONE', *, *, #12220, .T. ) ;
#12079 = VECTOR ( 'NONE', #6298, 1000.000000000000000 ) ;
#12080 = CARTESIAN_POINT ( 'NONE',  ( 0.6207106781186549904, 3.050000000000000266, 2.628553390593269423 ) ) ;
#12081 = EDGE_CURVE ( 'NONE', #5973, #11546, #5907, .T. ) ;
#12082 = CARTESIAN_POINT ( 'NONE',  ( 1.586727176531399941, -3.617010528270069969, 2.961885344765599726 ) ) ;
#12083 = EDGE_CURVE ( 'NONE', #1492, #7108, #4579, .T. ) ;
#12084 = DIRECTION ( 'NONE',  ( -1.000000000000000000, 1.480297366166879989E-15, 0.000000000000000000 ) ) ;
#12085 = LINE ( 'NONE', #3451, #15831 ) ;
#12086 = VECTOR ( 'NONE', #16862, 1000.000000000000000 ) ;
#12087 = CARTESIAN_POINT ( 'NONE',  ( 0.3681613504764975620, -3.477280798540335560, 2.680257674196191431 ) ) ;
#12088 = AXIS2_PLACEMENT_3D ( 'NONE', #1681, #5936, #814 ) ;
#12089 = CARTESIAN_POINT ( 'NONE',  ( 6.661338147750939243E-16, 1.250000000000000000, -1.318389841742369940E-16 ) ) ;
#12090 = LINE ( 'NONE', #17708, #12989 ) ;
#12091 = CARTESIAN_POINT ( 'NONE',  ( -1.835037444103819970, -1.358046564306109261, 5.620619042473610882 ) ) ;
#12092 = ORIENTED_EDGE ( 'NONE', *, *, #4253, .T. ) ;
#12093 = DIRECTION ( 'NONE',  ( 4.440892098500620245E-16, 1.000000000000000000, 1.110223024625159992E-16 ) ) ;
#12094 =( GEOMETRIC_REPRESENTATION_CONTEXT ( 3 ) GLOBAL_UNCERTAINTY_ASSIGNED_CONTEXT ( ( #6585 ) ) GLOBAL_UNIT_ASSIGNED_CONTEXT ( ( #12259, #17877, #11241 ) ) REPRESENTATION_CONTEXT ( 'NONE', 'WORKASPACE' ) );
#12095 = CARTESIAN_POINT ( 'NONE',  ( 1.159526867004269768, -0.4480353997208165184, 2.996084454861921209 ) ) ;
#12096 = CARTESIAN_POINT ( 'NONE',  ( -1.152986057740030379, -1.753947465207011058, 2.309657588616440549 ) ) ;
#12097 = ORIENTED_EDGE ( 'NONE', *, *, #12654, .F. ) ;
#12098 = LINE ( 'NONE', #3651, #11447 ) ;
#12099 = CARTESIAN_POINT ( 'NONE',  ( 2.287919158821199783, -1.051457940198389895, 5.251517552016890633 ) ) ;
#12100 = DIRECTION ( 'NONE',  ( 0.000000000000000000, 0.000000000000000000, -1.000000000000000000 ) ) ;
#12101 = CARTESIAN_POINT ( 'NONE',  ( -2.253200202764409799, -5.211016949152540434, 5.379408587037509903 ) ) ;
#12102 = ORIENTED_EDGE ( 'NONE', *, *, #6311, .T. ) ;
#12103 =( BOUNDED_SURFACE ( )  B_SPLINE_SURFACE ( 3, 3, ( 
 ( #4926, #12170, #3633, #14946, #10774, #6404, #12075, #8183, #17697, #5323, #5029, #15229, #10685, #2257, #9190, #10969, #10584, #773, #13558, #7809, #7907, #873, #16523, #16237, #6513, #3833, #12447, #16418, #3725, #9383, #8100, #2360, #3914, #6697, #12260, #16614, #13654, #12354, #3543, #6602, #9481, #2533, #15141, #13832, #1152, #6799, #2453, #13739, #17978, #2817, #18064, #16696, #8459, #1614, #3005, #9853, #12622, #12728, #14096, #15328, #4376, #18246 ),
 ( #2636, #5597, #5689, #1326, #16790, #11334, #4105, #17054, #7258, #5407, #11046, #12532, #8285, #1427, #4004, #11242, #4282, #15425, #9658, #13927, #9939, #1244, #2732, #8378, #7085, #14012, #11420, #16886, #6973, #46, #14293, #16970, #6886, #15512, #18145, #4193, #15599, #8560, #5493, #11136, #2912, #9760, #14206, #12816, #1527, #7176, #128, #5778, #10038, #15694, #8646, #17498, #14557, #578, #3170, #7439, #10384, #8989, #15966, #10299, #5953, #2048 ),
 ( #11593, #3267, #1871, #8909, #7520, #11511, #17141, #15861, #4544, #313, #6127, #4465, #11790, #10123, #15777, #6039, #16046, #12901, #10197, #13164, #13080, #1795, #480, #17412, #14372, #3344, #9074, #400, #4816, #3085, #14638, #7351, #8728, #4734, #11685, #4639, #1699, #17311, #1951, #14477, #17222, #7609, #8827, #11878, #223, #5864, #12993, #13258, #6219, #10466, #16126, #3423, #14734, #5017, #13349, #16221, #12242, #3528, #10669, #16315, #3708, #3620 ),
 ( #15126, #9270, #17774, #16404, #12335, #10950, #663, #14931, #17573, #9554, #950, #857, #9173, #13443, #13725, #753, #2150, #15029, #10852, #9464, #6497, #6387, #12156, #17862, #16597, #6301, #17957, #11960, #7795, #5200, #15213, #7703, #16500, #7993, #12058, #17678, #2241, #5107, #9358, #10759, #2344, #4907, #10562, #7885, #13539, #13639, #6588, #14835, #3814, #2439, #8086, #1041, #6677, #5303, #3900, #12428, #6781, #2794, #2520, #4081, #8438, #10016 ),
 ( #5668, #12514, #1502, #4257, #9831, #8536, #13988, #16947, #13808, #8167, #1398, #14186, #2706, #7157, #5754, #12794, #1221, #1133, #18047, #1306, #11310, #5391, #11031, #16679, #3987, #14072, #9636, #9740, #7065, #15303, #8355, #15403, #2615, #9916, #18127, #107, #15574, #15487, #11396, #6952, #2886, #8266, #13907, #12706, #17028, #12598, #4351, #6867, #5476, #11116, #16763, #23, #5574, #18219, #11219, #16863, #4170, #801, #7415, #10176, #10268, #376 ),
 ( #4610, #15840, #13056, #12877, #3139, #3242, #17201, #14347, #8885, #1672, #14881, #5060, #15676, #2985, #10104, #191, #17284, #8627, #8797, #2096, #12968, #14269, #5836, #7747, #11488, #292, #5930, #11660, #11570, #9217, #14448, #4525, #15937, #12111, #14535, #1592, #6016, #17120, #1768, #13393, #6342, #15755, #3062, #707, #7322, #12006, #10618, #4444, #17624, #17730, #4963, #16267, #3570, #2195, #7839, #13486, #6442, #7234, #8705, #8213, #6827, #13761 ),
 ( #10993, #5151, #2395, #3758, #8125, #12383, #1083, #6729, #9311, #14980, #13685, #8043, #16447, #3943, #2291, #9598, #993, #9419, #18005, #5349, #16641, #15254, #7944, #13592, #6630, #12287, #15085, #2559, #907, #13860, #6545, #12198, #3859, #1179, #10711, #17814, #10801, #17908, #12471, #16357, #5249, #18089, #18171, #16552, #10905, #9512, #5436, #15170, #9685, #11076, #16720, #4031, #2481, #15356, #3662, #2660, #8313, #13951, #1268, #6912, #12560, #15795 ) ),
 .UNSPECIFIED., .T., .F., .F. ) 
 B_SPLINE_SURFACE_WITH_KNOTS ( ( 4, 3, 4 ),
 ( 4, 1, 1, 1, 1, 1, 1, 1, 1, 1, 1, 1, 1, 1, 1, 1, 1, 1, 1, 1, 1, 1, 1, 1, 1, 1, 1, 1, 1, 1, 1, 1, 1, 1, 1, 1, 1, 1, 1, 1, 1, 1, 1, 1, 1, 1, 1, 1, 1, 1, 1, 1, 1, 1, 1, 1, 1, 1, 1, 4 ),
 ( 0.000000000000000000, 3.141592653589790007, 6.283185307179590673 ),
 ( 0.7853981633974479459, 0.8785809963429079827, 0.9717638292883680196, 1.064946662233830166, 1.158129495179289981, 1.251312328124750017, 1.344495161070210054, 1.437677994015669869, 1.530860826961130128, 1.624043659906589943, 1.717226492852049979, 1.810409325797510016, 1.903592158742969831, 1.996774991688430090, 2.089957824633889683, 2.183140657579349941, 2.276323490524809756, 2.369506323470270015, 2.462689156415730274, 2.555871989361190089, 2.649054822306649903, 2.742237655252109718, 2.835420488197569977, 2.928603321143030236, 3.021786154088490051, 3.114968987033949865, 3.208151819979410124, 3.301334652924869939, 3.394517485870330198, 3.487700318815790013, 3.580883151761249827, 3.674065984706710086, 3.767248817652169901, 3.860431650597620390, 3.953614483543080205, 4.046797316488540019, 4.139980149433999834, 4.233162982379460537, 4.326345815324920352, 4.419528648270380167, 4.512711481215839981, 4.605894314161299796, 4.699077147106759611, 4.792259980052219426, 4.885442812997680129, 4.978625645943139943, 5.071808478888599758, 5.164991311834059573, 5.258174144779520276, 5.351356977724980091, 5.444539810670439905, 5.537722643615899720, 5.630905476561360423, 5.724088309506820238, 5.817271142452280053, 5.910453975397739868, 6.003636808343199682, 6.096819641288659497, 6.190002474234119312, 6.283185307179590673 ),
 .UNSPECIFIED. ) 
 GEOMETRIC_REPRESENTATION_ITEM ( )  RATIONAL_B_SPLINE_SURFACE ( (
 ( 1.000000000000000000, 1.000000000000000000, 1.000000000000000000, 1.000000000000000000, 1.000000000000000000, 1.000000000000000000, 1.000000000000000000, 1.000000000000000000, 1.000000000000000000, 1.000000000000000000, 1.000000000000000000, 1.000000000000000000, 1.000000000000000000, 1.000000000000000000, 1.000000000000000000, 1.000000000000000000, 1.000000000000000000, 1.000000000000000000, 1.000000000000000000, 1.000000000000000000, 1.000000000000000000, 1.000000000000000000, 1.000000000000000000, 1.000000000000000000, 1.000000000000000000, 1.000000000000000000, 1.000000000000000000, 1.000000000000000000, 1.000000000000000000, 1.000000000000000000, 1.000000000000000000, 1.000000000000000000, 1.000000000000000000, 1.000000000000000000, 1.000000000000000000, 1.000000000000000000, 1.000000000000000000, 1.000000000000000000, 1.000000000000000000, 1.000000000000000000, 1.000000000000000000, 1.000000000000000000, 1.000000000000000000, 1.000000000000000000, 1.000000000000000000, 1.000000000000000000, 1.000000000000000000, 1.000000000000000000, 1.000000000000000000, 1.000000000000000000, 1.000000000000000000, 1.000000000000000000, 1.000000000000000000, 1.000000000000000000, 1.000000000000000000, 1.000000000000000000, 1.000000000000000000, 1.000000000000000000, 1.000000000000000000, 1.000000000000000000, 1.000000000000000000, 1.000000000000000000),
 ( 0.3333333333333329818, 0.3333333333333329818, 0.3333333333333329818, 0.3333333333333329818, 0.3333333333333329818, 0.3333333333333329818, 0.3333333333333329818, 0.3333333333333329818, 0.3333333333333329818, 0.3333333333333329818, 0.3333333333333329818, 0.3333333333333329818, 0.3333333333333329818, 0.3333333333333329818, 0.3333333333333329818, 0.3333333333333329818, 0.3333333333333329818, 0.3333333333333329818, 0.3333333333333329818, 0.3333333333333329818, 0.3333333333333329818, 0.3333333333333329818, 0.3333333333333329818, 0.3333333333333329818, 0.3333333333333329818, 0.3333333333333329818, 0.3333333333333329818, 0.3333333333333329818, 0.3333333333333329818, 0.3333333333333329818, 0.3333333333333329818, 0.3333333333333329818, 0.3333333333333329818, 0.3333333333333329818, 0.3333333333333329818, 0.3333333333333329818, 0.3333333333333329818, 0.3333333333333329818, 0.3333333333333329818, 0.3333333333333329818, 0.3333333333333329818, 0.3333333333333329818, 0.3333333333333329818, 0.3333333333333329818, 0.3333333333333329818, 0.3333333333333329818, 0.3333333333333329818, 0.3333333333333329818, 0.3333333333333329818, 0.3333333333333329818, 0.3333333333333329818, 0.3333333333333329818, 0.3333333333333329818, 0.3333333333333329818, 0.3333333333333329818, 0.3333333333333329818, 0.3333333333333329818, 0.3333333333333329818, 0.3333333333333329818, 0.3333333333333329818, 0.3333333333333329818, 0.3333333333333329818),
 ( 0.3333333333333329818, 0.3333333333333329818, 0.3333333333333329818, 0.3333333333333329818, 0.3333333333333329818, 0.3333333333333329818, 0.3333333333333329818, 0.3333333333333329818, 0.3333333333333329818, 0.3333333333333329818, 0.3333333333333329818, 0.3333333333333329818, 0.3333333333333329818, 0.3333333333333329818, 0.3333333333333329818, 0.3333333333333329818, 0.3333333333333329818, 0.3333333333333329818, 0.3333333333333329818, 0.3333333333333329818, 0.3333333333333329818, 0.3333333333333329818, 0.3333333333333329818, 0.3333333333333329818, 0.3333333333333329818, 0.3333333333333329818, 0.3333333333333329818, 0.3333333333333329818, 0.3333333333333329818, 0.3333333333333329818, 0.3333333333333329818, 0.3333333333333329818, 0.3333333333333329818, 0.3333333333333329818, 0.3333333333333329818, 0.3333333333333329818, 0.3333333333333329818, 0.3333333333333329818, 0.3333333333333329818, 0.3333333333333329818, 0.3333333333333329818, 0.3333333333333329818, 0.3333333333333329818, 0.3333333333333329818, 0.3333333333333329818, 0.3333333333333329818, 0.3333333333333329818, 0.3333333333333329818, 0.3333333333333329818, 0.3333333333333329818, 0.3333333333333329818, 0.3333333333333329818, 0.3333333333333329818, 0.3333333333333329818, 0.3333333333333329818, 0.3333333333333329818, 0.3333333333333329818, 0.3333333333333329818, 0.3333333333333329818, 0.3333333333333329818, 0.3333333333333329818, 0.3333333333333329818),
 ( 1.000000000000000000, 1.000000000000000000, 1.000000000000000000, 1.000000000000000000, 1.000000000000000000, 1.000000000000000000, 1.000000000000000000, 1.000000000000000000, 1.000000000000000000, 1.000000000000000000, 1.000000000000000000, 1.000000000000000000, 1.000000000000000000, 1.000000000000000000, 1.000000000000000000, 1.000000000000000000, 1.000000000000000000, 1.000000000000000000, 1.000000000000000000, 1.000000000000000000, 1.000000000000000000, 1.000000000000000000, 1.000000000000000000, 1.000000000000000000, 1.000000000000000000, 1.000000000000000000, 1.000000000000000000, 1.000000000000000000, 1.000000000000000000, 1.000000000000000000, 1.000000000000000000, 1.000000000000000000, 1.000000000000000000, 1.000000000000000000, 1.000000000000000000, 1.000000000000000000, 1.000000000000000000, 1.000000000000000000, 1.000000000000000000, 1.000000000000000000, 1.000000000000000000, 1.000000000000000000, 1.000000000000000000, 1.000000000000000000, 1.000000000000000000, 1.000000000000000000, 1.000000000000000000, 1.000000000000000000, 1.000000000000000000, 1.000000000000000000, 1.000000000000000000, 1.000000000000000000, 1.000000000000000000, 1.000000000000000000, 1.000000000000000000, 1.000000000000000000, 1.000000000000000000, 1.000000000000000000, 1.000000000000000000, 1.000000000000000000, 1.000000000000000000, 1.000000000000000000),
 ( 0.3333333333333329818, 0.3333333333333329818, 0.3333333333333329818, 0.3333333333333329818, 0.3333333333333329818, 0.3333333333333329818, 0.3333333333333329818, 0.3333333333333329818, 0.3333333333333329818, 0.3333333333333329818, 0.3333333333333329818, 0.3333333333333329818, 0.3333333333333329818, 0.3333333333333329818, 0.3333333333333329818, 0.3333333333333329818, 0.3333333333333329818, 0.3333333333333329818, 0.3333333333333329818, 0.3333333333333329818, 0.3333333333333329818, 0.3333333333333329818, 0.3333333333333329818, 0.3333333333333329818, 0.3333333333333329818, 0.3333333333333329818, 0.3333333333333329818, 0.3333333333333329818, 0.3333333333333329818, 0.3333333333333329818, 0.3333333333333329818, 0.3333333333333329818, 0.3333333333333329818, 0.3333333333333329818, 0.3333333333333329818, 0.3333333333333329818, 0.3333333333333329818, 0.3333333333333329818, 0.3333333333333329818, 0.3333333333333329818, 0.3333333333333329818, 0.3333333333333329818, 0.3333333333333329818, 0.3333333333333329818, 0.3333333333333329818, 0.3333333333333329818, 0.3333333333333329818, 0.3333333333333329818, 0.3333333333333329818, 0.3333333333333329818, 0.3333333333333329818, 0.3333333333333329818, 0.3333333333333329818, 0.3333333333333329818, 0.3333333333333329818, 0.3333333333333329818, 0.3333333333333329818, 0.3333333333333329818, 0.3333333333333329818, 0.3333333333333329818, 0.3333333333333329818, 0.3333333333333329818),
 ( 0.3333333333333329818, 0.3333333333333329818, 0.3333333333333329818, 0.3333333333333329818, 0.3333333333333329818, 0.3333333333333329818, 0.3333333333333329818, 0.3333333333333329818, 0.3333333333333329818, 0.3333333333333329818, 0.3333333333333329818, 0.3333333333333329818, 0.3333333333333329818, 0.3333333333333329818, 0.3333333333333329818, 0.3333333333333329818, 0.3333333333333329818, 0.3333333333333329818, 0.3333333333333329818, 0.3333333333333329818, 0.3333333333333329818, 0.3333333333333329818, 0.3333333333333329818, 0.3333333333333329818, 0.3333333333333329818, 0.3333333333333329818, 0.3333333333333329818, 0.3333333333333329818, 0.3333333333333329818, 0.3333333333333329818, 0.3333333333333329818, 0.3333333333333329818, 0.3333333333333329818, 0.3333333333333329818, 0.3333333333333329818, 0.3333333333333329818, 0.3333333333333329818, 0.3333333333333329818, 0.3333333333333329818, 0.3333333333333329818, 0.3333333333333329818, 0.3333333333333329818, 0.3333333333333329818, 0.3333333333333329818, 0.3333333333333329818, 0.3333333333333329818, 0.3333333333333329818, 0.3333333333333329818, 0.3333333333333329818, 0.3333333333333329818, 0.3333333333333329818, 0.3333333333333329818, 0.3333333333333329818, 0.3333333333333329818, 0.3333333333333329818, 0.3333333333333329818, 0.3333333333333329818, 0.3333333333333329818, 0.3333333333333329818, 0.3333333333333329818, 0.3333333333333329818, 0.3333333333333329818),
 ( 1.000000000000000000, 1.000000000000000000, 1.000000000000000000, 1.000000000000000000, 1.000000000000000000, 1.000000000000000000, 1.000000000000000000, 1.000000000000000000, 1.000000000000000000, 1.000000000000000000, 1.000000000000000000, 1.000000000000000000, 1.000000000000000000, 1.000000000000000000, 1.000000000000000000, 1.000000000000000000, 1.000000000000000000, 1.000000000000000000, 1.000000000000000000, 1.000000000000000000, 1.000000000000000000, 1.000000000000000000, 1.000000000000000000, 1.000000000000000000, 1.000000000000000000, 1.000000000000000000, 1.000000000000000000, 1.000000000000000000, 1.000000000000000000, 1.000000000000000000, 1.000000000000000000, 1.000000000000000000, 1.000000000000000000, 1.000000000000000000, 1.000000000000000000, 1.000000000000000000, 1.000000000000000000, 1.000000000000000000, 1.000000000000000000, 1.000000000000000000, 1.000000000000000000, 1.000000000000000000, 1.000000000000000000, 1.000000000000000000, 1.000000000000000000, 1.000000000000000000, 1.000000000000000000, 1.000000000000000000, 1.000000000000000000, 1.000000000000000000, 1.000000000000000000, 1.000000000000000000, 1.000000000000000000, 1.000000000000000000, 1.000000000000000000, 1.000000000000000000, 1.000000000000000000, 1.000000000000000000, 1.000000000000000000, 1.000000000000000000, 1.000000000000000000, 1.000000000000000000) ) ) 
 REPRESENTATION_ITEM ( '' )  SURFACE ( )  );
#12104 = ORIENTED_EDGE ( 'NONE', *, *, #1887, .F. ) ;
#12105 = CARTESIAN_POINT ( 'NONE',  ( -1.899999999999999911, 8.500000000000000000, 0.6099999999999999867 ) ) ;
#12106 = PLANE ( 'NONE',  #16200 ) ;
#12107 = AXIS2_PLACEMENT_3D ( 'NONE', #7749, #16449, #8046 ) ;
#12108 = CARTESIAN_POINT ( 'NONE',  ( 1.399999999999999911, 0.5999999999999999778, 3.299999999999999822 ) ) ;
#12109 = EDGE_CURVE ( 'NONE', #6911, #9328, #6255, .T. ) ;
#12110 = EDGE_LOOP ( 'NONE', ( #18214, #17337, #7579, #17261 ) ) ;
#12111 = CARTESIAN_POINT ( 'NONE',  ( -1.202278654260740876, -5.479872881355935199, 6.364093491318035589 ) ) ;
#12112 = CARTESIAN_POINT ( 'NONE',  ( -2.398725280367459245, -3.151244762504313179, 3.564557036955213754 ) ) ;
#12113 = CARTESIAN_POINT ( 'NONE',  ( 1.850000000000000089, 0.7500000000000000000, 7.649999999999999467 ) ) ;
#12114 = CARTESIAN_POINT ( 'NONE',  ( -1.700860513939528751, -3.124115597856051085, 6.737200825918551850 ) ) ;
#12115 = LINE ( 'NONE', #2005, #5276 ) ;
#12116 = DIRECTION ( 'NONE',  ( 0.000000000000000000, -1.000000000000000000, 0.000000000000000000 ) ) ;
#12117 = CARTESIAN_POINT ( 'NONE',  ( -1.928817277882840076, -4.455388906648449776, 6.048484184565969812 ) ) ;
#12118 = CARTESIAN_POINT ( 'NONE',  ( -1.000000000000000000, 5.400000000000000355, 7.700000000000000178 ) ) ;
#12119 = CARTESIAN_POINT ( 'NONE',  ( -2.500000000000000000, 4.700000000000000178, 0.5999999999999999778 ) ) ;
#12120 = ADVANCED_FACE ( 'NONE', ( #11914 ), #5993, .F. ) ;
#12122 = ORIENTED_EDGE ( 'NONE', *, *, #4388, .T. ) ;
#12121 = CARTESIAN_POINT ( 'NONE',  ( -1.963178672446121098, -1.959701183441630024, 2.914210764660470687 ) ) ;
#12123 = DIRECTION ( 'NONE',  ( 2.220446049250309876E-16, 0.000000000000000000, 1.000000000000000000 ) ) ;
#12124 = LINE ( 'NONE', #17548, #4624 ) ;
#12125 = CARTESIAN_POINT ( 'NONE',  ( 1.928817277882869829, -1.144611093351550091, 6.048484184565929844 ) ) ;
#12126 = LINE ( 'NONE', #12214, #12496 ) ;
#12127 = LINE ( 'NONE', #5077, #9150 ) ;
#12128 = CARTESIAN_POINT ( 'NONE',  ( -1.248294325655370018, -5.573305084745760141, 2.704938983774309857 ) ) ;
#12129 = ORIENTED_EDGE ( 'NONE', *, *, #2700, .T. ) ;
#12130 = FACE_OUTER_BOUND ( 'NONE', #16049, .T. ) ;
#12131 = CARTESIAN_POINT ( 'NONE',  ( 3.673940397442059498E-17, 3.581751045813930112, 8.000000000000000000 ) ) ;
#12132 = EDGE_CURVE ( 'NONE', #6275, #6036, #6077, .T. ) ;
#12133 = ORIENTED_EDGE ( 'NONE', *, *, #17389, .F. ) ;
#12134 = AXIS2_PLACEMENT_3D ( 'NONE', #6746, #12398, #18017 ) ;
#12135 = CARTESIAN_POINT ( 'NONE',  ( 1.832842064134690085, -2.728214696955149954, 6.176291182464479945 ) ) ;
#12136 = DIRECTION ( 'NONE',  ( -7.092954723563668294E-17, -0.8944271909999148562, -0.4472135954999599261 ) ) ;
#12137 = CARTESIAN_POINT ( 'NONE',  ( -1.057242234132100167, -5.577754237288139905, 2.597442975781530272 ) ) ;
#12138 = CARTESIAN_POINT ( 'NONE',  ( 1.000000000000000000, -6.000000000000000000, 5.100000000000000533 ) ) ;
#12139 = CARTESIAN_POINT ( 'NONE',  ( -1.044181395669830259, -2.052854336594790219, 2.590869634085910089 ) ) ;
#12140 = CARTESIAN_POINT ( 'NONE',  ( 0.5500000000000000444, -2.399999999999999911, 3.600000000000000089 ) ) ;
#12141 = CARTESIAN_POINT ( 'NONE',  ( -1.978802102381380879, -1.843259742000191048, 4.152967933079680485 ) ) ;
#12142 = CARTESIAN_POINT ( 'NONE',  ( 1.194742379459969861, -0.4245762711864409789, 6.727584234649759409 ) ) ;
#12143 = DIRECTION ( 'NONE',  ( 0.000000000000000000, -1.000000000000000000, 0.000000000000000000 ) ) ;
#12144 = CARTESIAN_POINT ( 'NONE',  ( -0.8740908734716290596, 4.154758922476410099, 7.700000000000000178 ) ) ;
#12145 = ORIENTED_EDGE ( 'NONE', *, *, #15265, .F. ) ;
#12146 = CARTESIAN_POINT ( 'NONE',  ( 1.553986151955640160, -0.6610754142986889903, 3.144168668454419890 ) ) ;
#12147 = LINE ( 'NONE', #13801, #5461 ) ;
#12148 = CARTESIAN_POINT ( 'NONE',  ( 1.994983296312400123, -4.265241723982169830, 5.948514050749290405 ) ) ;
#12149 = ORIENTED_EDGE ( 'NONE', *, *, #16050, .T. ) ;
#12150 = ORIENTED_EDGE ( 'NONE', *, *, #5296, .T. ) ;
#12151 = CARTESIAN_POINT ( 'NONE',  ( 0.1749999999999999889, 8.800000000000000711, 0.4000000000000000222 ) ) ;
#12152 = ADVANCED_FACE ( 'NONE', ( #17533 ), #4861, .T. ) ;
#12153 = ORIENTED_EDGE ( 'NONE', *, *, #11572, .F. ) ;
#12154 = DIRECTION ( 'NONE',  ( 0.000000000000000000, 0.000000000000000000, 1.000000000000000000 ) ) ;
#12155 = PRODUCT_CONTEXT ( 'NONE', #8745, 'mechanical' ) ;
#12156 = CARTESIAN_POINT ( 'NONE',  ( 0.9150601050661639757, -5.130932203389829915, 6.868218666554230190 ) ) ;
#12157 = PRODUCT_DEFINITION_SHAPE ( 'NONE', 'NONE',  #18300 ) ;
#12158 = VECTOR ( 'NONE', #7272, 1000.000000000000000 ) ;
#12159 = CARTESIAN_POINT ( 'NONE',  ( 3.371799150351489833E-16, 2.299999999999999822, 7.599999999999999645 ) ) ;
#12160 = VERTEX_POINT ( 'NONE', #14777 ) ;
#12161 = CARTESIAN_POINT ( 'NONE',  ( -2.260890494820599894, -1.544352870612419881, 4.046455925041199997 ) ) ;
#12162 = FACE_OUTER_BOUND ( 'NONE', #14512, .T. ) ;
#12163 = CARTESIAN_POINT ( 'NONE',  ( -1.117157304995339606, -4.661142624883069630, 6.422457952614126775 ) ) ;
#12164 = CARTESIAN_POINT ( 'NONE',  ( 0.5889081234606849957, -0.1379237288135600203, 6.978529000034869867 ) ) ;
#12165 = VERTEX_POINT ( 'NONE', #3472 ) ;
#12166 = CARTESIAN_POINT ( 'NONE',  ( -2.191755591049691532, -0.2536016949152540834, 3.203650300307721466 ) ) ;
#12167 = VERTEX_POINT ( 'NONE', #13031 ) ;
#12168 = CARTESIAN_POINT ( 'NONE',  ( -0.6493550500446439999, -5.586652542372879005, 2.437955526623099889 ) ) ;
#12169 = CARTESIAN_POINT ( 'NONE',  ( -1.994983296312368815, -1.334758276017820045, 5.948514050749341919 ) ) ;
#12170 = CARTESIAN_POINT ( 'NONE',  ( 1.713314936023349944, -5.338983050847460277, 3.089913064446569546 ) ) ;
#12171 = CARTESIAN_POINT ( 'NONE',  ( 1.835211330903820937, -0.8922807985403484743, 6.617058440403981834 ) ) ;
#12172 = VERTEX_POINT ( 'NONE', #3307 ) ;
#12173 = CARTESIAN_POINT ( 'NONE',  ( -1.505092429369619955, -5.128627060139309357, 2.879659483602799774 ) ) ;
#12174 = CARTESIAN_POINT ( 'NONE',  ( 0.3752419433107369584, -4.175929447188989840, 7.023346545710360544 ) ) ;
#12175 = CARTESIAN_POINT ( 'NONE',  ( 0.9279264017968674727, -4.428259742000194343, 7.186376135231798301 ) ) ;
#12176 = FACE_OUTER_BOUND ( 'NONE', #11875, .T. ) ;
#12177 = CARTESIAN_POINT ( 'NONE',  ( -1.750000000000000000, 11.40000000000000036, 7.700000000000000178 ) ) ;
#12178 = CARTESIAN_POINT ( 'NONE',  ( -1.292934267244330471, -4.385524041783587457, 6.294748514096648151 ) ) ;
#12179 = CARTESIAN_POINT ( 'NONE',  ( 0.5500000000000000444, 2.050000000000000266, 3.600000000000000089 ) ) ;
#12180 = CARTESIAN_POINT ( 'NONE',  ( -2.053018524985070314, -1.474488005747551567, 4.695903819313384631 ) ) ;
#12181 = ORIENTED_EDGE ( 'NONE', *, *, #7917, .F. ) ;
#12182 = LINE ( 'NONE', #365, #2457 ) ;
#12183 = CARTESIAN_POINT ( 'NONE',  ( 6.735557395310439065E-16, -5.500000000000000000, -3.367778697655220026E-16 ) ) ;
#12184 = EDGE_CURVE ( 'NONE', #14849, #15379, #9120, .T. ) ;
#12185 = CARTESIAN_POINT ( 'NONE',  ( -1.399999999999999911, -8.000000000000000000, 6.100000000000000533 ) ) ;
#12186 = CARTESIAN_POINT ( 'NONE',  ( 2.435897774776379698, -2.359442960702510472, 5.753335522918191280 ) ) ;
#12187 = ADVANCED_FACE ( 'NONE', ( #14513 ), #12942, .T. ) ;
#12188 = VERTEX_POINT ( 'NONE', #7477 ) ;
#12189 = DIRECTION ( 'NONE',  ( -1.000000000000000000, -1.168655815394900078E-16, -1.168655815394900078E-16 ) ) ;
#12190 = PLANE ( 'NONE',  #4149 ) ;
#12191 = CARTESIAN_POINT ( 'NONE',  ( 1.782460458101500889, -5.099788135593215976, 5.718585207845976015 ) ) ;
#12192 = ORIENTED_EDGE ( 'NONE', *, *, #13109, .T. ) ;
#12193 = ORIENTED_EDGE ( 'NONE', *, *, #16713, .F. ) ;
#12194 = CARTESIAN_POINT ( 'NONE',  ( 1.899999999999999911, 11.29999999999999893, 7.649999999999999467 ) ) ;
#12195 = LINE ( 'NONE', #9026, #523 ) ;
#12196 = CARTESIAN_POINT ( 'NONE',  ( 1.399999999999999911, -8.000000000000000000, 6.100000000000000533 ) ) ;
#12197 = VERTEX_POINT ( 'NONE', #17360 ) ;
#12198 = CARTESIAN_POINT ( 'NONE',  ( -1.000896394980330006, -5.470974576271190770, 6.829956240957379521 ) ) ;
#12199 = CARTESIAN_POINT ( 'NONE',  ( -1.853635285637788899, -4.408812330071866015, 6.599249831075526984 ) ) ;
#12200 = DIRECTION ( 'NONE',  ( 0.000000000000000000, -1.000000000000000000, 0.000000000000000000 ) ) ;
#12201 = PLANE ( 'NONE',  #1717 ) ;
#12202 = DIRECTION ( 'NONE',  ( -1.556829778943089964E-16, 0.000000000000000000, 1.000000000000000000 ) ) ;
#12203 = CARTESIAN_POINT ( 'NONE',  ( -2.046174187462380445, -4.478677194936739880, 5.862719605944009871 ) ) ;
#12204 = DIRECTION ( 'NONE',  ( -4.318427418585891014E-15, 2.220446049250309876E-16, -1.000000000000000000 ) ) ;
#12205 = EDGE_CURVE ( 'NONE', #9633, #14829, #269, .T. ) ;
#12206 = LINE ( 'NONE', #2302, #7378 ) ;
#12208 = ORIENTED_EDGE ( 'NONE', *, *, #14645, .T. ) ;
#12207 = CARTESIAN_POINT ( 'NONE',  ( 2.398725280367429047, -2.448755237495690462, 3.564557036955152913 ) ) ;
#12209 = EDGE_CURVE ( 'NONE', #11655, #2611, #17443, .T. ) ;
#12210 = DIRECTION ( 'NONE',  ( 0.000000000000000000, 0.000000000000000000, -1.000000000000000000 ) ) ;
#12211 = CARTESIAN_POINT ( 'NONE',  ( 1.438959988998139914E-16, -0.2999999999999999889, 2.350000000000000089 ) ) ;
#12212 = EDGE_CURVE ( 'NONE', #8376, #11415, #7394, .T. ) ;
#12213 = CARTESIAN_POINT ( 'NONE',  ( 1.611907055891590002, -2.355602084342530045, 2.985210995296850189 ) ) ;
#12214 = CARTESIAN_POINT ( 'NONE',  ( 1.899999999999999911, 0.5999999999999999778, 0.5999999999999999778 ) ) ;
#12215 = CARTESIAN_POINT ( 'NONE',  ( 1.828929293328490072E-16, 2.399999999999999911, 5.100000000000000533 ) ) ;
#12216 = CARTESIAN_POINT ( 'NONE',  ( -2.306642602145299925, -5.515466101694909362, 5.166805192608490138 ) ) ;
#12217 = ORIENTED_EDGE ( 'NONE', *, *, #6476, .T. ) ;
#12218 = LINE ( 'NONE', #11010, #10221 ) ;
#12219 = CARTESIAN_POINT ( 'NONE',  ( 0.009417288784633505092, -0.3007439470567257467, 2.370019840861780303 ) ) ;
#12220 = EDGE_CURVE ( 'NONE', #12458, #14546, #4687, .T. ) ;
#12221 = ORIENTED_EDGE ( 'NONE', *, *, #13436, .F. ) ;
#12222 = CARTESIAN_POINT ( 'NONE',  ( 1.397172971746949877, -3.892629111369559691, 2.806153814454899642 ) ) ;
#12223 = EDGE_CURVE ( 'NONE', #4252, #4577, #13204, .T. ) ;
#12224 = CARTESIAN_POINT ( 'NONE',  ( 0.1749999999999999889, 9.199999999999999289, 0.4000000000000000222 ) ) ;
#12225 = CARTESIAN_POINT ( 'NONE',  ( -0.2189795514005259958, -5.595550847457629651, 2.356806637999020015 ) ) ;
#12226 = CARTESIAN_POINT ( 'NONE',  ( -2.500000000000000000, 7.299999999999999822, 1.600000000000000089 ) ) ;
#12227 = CARTESIAN_POINT ( 'NONE',  ( -0.5320716618283710675, -3.007674156414609890, 6.992519451207139802 ) ) ;
#12228 = CARTESIAN_POINT ( 'NONE',  ( -1.670747221194380128, -5.103620102360550526, 3.047345349617600174 ) ) ;
#12229 = CARTESIAN_POINT ( 'NONE',  ( -1.491388273268980491, -1.587088570829020551, 6.110908523251552538 ) ) ;
#12230 = EDGE_CURVE ( 'NONE', #9094, #14730, #9025, .T. ) ;
#12231 = DIRECTION ( 'NONE',  ( -1.899065700016719806E-16, -1.000000000000000000, 0.000000000000000000 ) ) ;
#12232 = CARTESIAN_POINT ( 'NONE',  ( -0.2097343361107079085, -0.5962015548080615845, 2.050670208512068715 ) ) ;
#12233 = EDGE_LOOP ( 'NONE', ( #4709, #7451, #8551, #16887 ) ) ;
#12234 = CARTESIAN_POINT ( 'NONE',  ( 1.554908741750600232, -5.202797822590530252, 3.145091258249389732 ) ) ;
#12235 = PLANE ( 'NONE',  #8108 ) ;
#12236 = CARTESIAN_POINT ( 'NONE',  ( -2.239137794397029868, -4.987178660919110662, 3.975425900939220103 ) ) ;
#12237 = ORIENTED_EDGE ( 'NONE', *, *, #1694, .F. ) ;
#12238 = ORIENTED_EDGE ( 'NONE', *, *, #12855, .T. ) ;
#12239 = FACE_OUTER_BOUND ( 'NONE', #13869, .T. ) ;
#12240 = ORIENTED_EDGE ( 'NONE', *, *, #9955, .T. ) ;
#12241 = CARTESIAN_POINT ( 'NONE',  ( 0.3042893218813439438, 6.450000000000000178, 2.029289321881350361 ) ) ;
#12242 = CARTESIAN_POINT ( 'NONE',  ( -0.9664230948142090716, -5.282203389830510076, 2.228384861502259895 ) ) ;
#12243 = EDGE_CURVE ( 'NONE', #2692, #8647, #4772, .T. ) ;
#12244 = DIRECTION ( 'NONE',  ( -1.000000000000000000, 0.000000000000000000, 0.000000000000000000 ) ) ;
#12245 = CARTESIAN_POINT ( 'NONE',  ( 1.820241257191439921, -0.5196681859277348936, 3.208199930689769719 ) ) ;
#12246 = FACE_OUTER_BOUND ( 'NONE', #16059, .T. ) ;
#12247 = CARTESIAN_POINT ( 'NONE',  ( 2.329383452786330189, -1.028169651910100013, 5.035735636132829818 ) ) ;
#12248 = CARTESIAN_POINT ( 'NONE',  ( 1.889104232906359870, -0.04449152542372909747, 3.296507079072520163 ) ) ;
#12249 = EDGE_CURVE ( 'NONE', #3809, #16824, #606, .T. ) ;
#12250 = ORIENTED_EDGE ( 'NONE', *, *, #7833, .T. ) ;
#12251 = AXIS2_PLACEMENT_3D ( 'NONE', #8530, #14179, #1497 ) ;
#12252 = CARTESIAN_POINT ( 'NONE',  ( -1.940327948426050941, -0.5091101694915260989, 5.370677689277675526 ) ) ;
#12253 = ORIENTED_EDGE ( 'NONE', *, *, #9693, .F. ) ;
#12254 = CARTESIAN_POINT ( 'NONE',  ( -2.321479326063761395, -0.2491525423728809807, 3.414080590619972710 ) ) ;
#12255 = VERTEX_POINT ( 'NONE', #6338 ) ;
#12256 = LINE ( 'NONE', #12618, #15057 ) ;
#12257 = DIRECTION ( 'NONE',  ( -1.000000000000000000, 0.000000000000000000, 0.000000000000000000 ) ) ;
#12258 = CARTESIAN_POINT ( 'NONE',  ( -2.353452300571019506, -1.474488005747550456, 4.697179287168410156 ) ) ;
#12259 =( LENGTH_UNIT ( ) NAMED_UNIT ( * ) SI_UNIT ( .MILLI., .METRE. ) );
#12260 = CARTESIAN_POINT ( 'NONE',  ( -1.549742865090599997, -5.484322033898309634, 6.471102547561460305 ) ) ;
#12261 = CARTESIAN_POINT ( 'NONE',  ( -1.579331079541819394, -1.241605122864670285, 6.832797935622397567 ) ) ;
#12262 = ORIENTED_EDGE ( 'NONE', *, *, #536, .F. ) ;
#12263 = CARTESIAN_POINT ( 'NONE',  ( -0.1686436619862690112, -4.981295943764799894, 2.349239845786320391 ) ) ;
#12264 = CARTESIAN_POINT ( 'NONE',  ( 1.003115764947319910, -4.106064582324129297, 6.828967930617570126 ) ) ;
#12265 = LINE ( 'NONE', #10405, #3147 ) ;
#12266 = DIRECTION ( 'NONE',  ( -1.000000000000000000, 0.000000000000000000, 0.000000000000000000 ) ) ;
#12267 = ADVANCED_FACE ( 'NONE', ( #13679 ), #17725, .T. ) ;
#12268 = CARTESIAN_POINT ( 'NONE',  ( -1.919159680931840084, -1.866548030288480042, 3.970803207828165426 ) ) ;
#12269 = PLANE ( 'NONE',  #9374 ) ;
#12270 = CARTESIAN_POINT ( 'NONE',  ( 2.045969882616350155, -3.803316834576382366, 4.529973290172005562 ) ) ;
#12271 = ORIENTED_EDGE ( 'NONE', *, *, #14345, .T. ) ;
#12272 = LINE ( 'NONE', #6526, #11701 ) ;
#12273 = CARTESIAN_POINT ( 'NONE',  ( -0.7500000000000000000, 3.050000000000000266, 2.699264068711930253 ) ) ;
#12274 = CARTESIAN_POINT ( 'NONE',  ( -2.030998484741458832, -0.2180084745762719822, 4.999543428097190656 ) ) ;
#12275 = CARTESIAN_POINT ( 'NONE',  ( 1.458615186838411626, -0.4963798976394455664, 3.259477383973563125 ) ) ;
#12276 = CARTESIAN_POINT ( 'NONE',  ( 2.197904923864649529, -2.406019537279079579, 6.187389538303071923 ) ) ;
#12277 = VERTEX_POINT ( 'NONE', #5345 ) ;
#12278 = FACE_OUTER_BOUND ( 'NONE', #2558, .T. ) ;
#12279 = CARTESIAN_POINT ( 'NONE',  ( 4.265698758777729940E-16, 2.350000000000000089, 7.700000000000000178 ) ) ;
#12280 = CARTESIAN_POINT ( 'NONE',  ( -1.246151616534680651, -5.268855932203385883, 3.068501529594771071 ) ) ;
#12281 = EDGE_LOOP ( 'NONE', ( #4029, #2818, #1865 ) ) ;
#12282 = ORIENTED_EDGE ( 'NONE', *, *, #9492, .T. ) ;
#12283 = DIRECTION ( 'NONE',  ( 0.000000000000000000, 0.000000000000000000, -1.000000000000000000 ) ) ;
#12284 = CARTESIAN_POINT ( 'NONE',  ( 1.000000000000000000, -6.000000000000000000, 3.673738709727309981 ) ) ;
#12285 = FACE_OUTER_BOUND ( 'NONE', #374, .T. ) ;
#12286 = ORIENTED_EDGE ( 'NONE', *, *, #4348, .F. ) ;
#12287 = CARTESIAN_POINT ( 'NONE',  ( 0.2812789908084389889, -5.444279661016950378, 7.036533610117280624 ) ) ;
#12288 = CARTESIAN_POINT ( 'NONE',  ( 1.351547610267151533, -4.082776294035843634, 6.983951126925231456 ) ) ;
#12289 = CARTESIAN_POINT ( 'NONE',  ( 1.545075033357670158, -0.4774152569121719036, 2.920238509828300799 ) ) ;
#12290 = CARTESIAN_POINT ( 'NONE',  ( -2.589141052314440916, -3.287133615874059611, 5.282633936723525991 ) ) ;
#12291 = DIRECTION ( 'NONE',  ( 0.000000000000000000, 0.000000000000000000, -1.000000000000000000 ) ) ;
#12292 = ADVANCED_FACE ( 'NONE', ( #10901 ), #16637, .T. ) ;
#12293 = CARTESIAN_POINT ( 'NONE',  ( -0.7109160811435620841, -4.292370888630429704, 6.943511536198419876 ) ) ;
#12294 = CARTESIAN_POINT ( 'NONE',  ( -1.899999999999999911, 2.000000000000000000, 1.600000000000000089 ) ) ;
#12295 = CARTESIAN_POINT ( 'NONE',  ( -2.500000000000000000, 7.299999999999999822, 1.600000000000000089 ) ) ;
#12297 = ORIENTED_EDGE ( 'NONE', *, *, #4384, .F. ) ;
#12296 = CARTESIAN_POINT ( 'NONE',  ( -0.3578984759183553854, -2.984385868126320673, 7.329643012642057087 ) ) ;
#12298 = PLANE ( 'NONE',  #16517 ) ;
#12299 = CARTESIAN_POINT ( 'NONE',  ( 2.318251751302029984, -0.3667372881355940306, 4.294764266798990704 ) ) ;
#12300 = CARTESIAN_POINT ( 'NONE',  ( -1.044181395669830259, -2.052854336594790219, 2.590869634085910089 ) ) ;
#12301 = CARTESIAN_POINT ( 'NONE',  ( -1.300961508564169922, -0.4779661016949160457, 6.661123742937279602 ) ) ;
#12302 = CARTESIAN_POINT ( 'NONE',  ( -2.011500846714319835, -5.551059322033900401, 3.478373409938470218 ) ) ;
#12303 = VERTEX_POINT ( 'NONE', #8038 ) ;
#12304 = DIRECTION ( 'NONE',  ( 0.000000000000000000, 1.000000000000000000, -1.110223024625159745E-16 ) ) ;
#12305 = ORIENTED_EDGE ( 'NONE', *, *, #14060, .T. ) ;
#12306 = CARTESIAN_POINT ( 'NONE',  ( -1.194742379459959869, -5.175423728813559165, 6.727584234649758521 ) ) ;
#12307 = DIRECTION ( 'NONE',  ( 0.7071067811865489050, 0.000000000000000000, -0.7071067811865461294 ) ) ;
#12308 = CARTESIAN_POINT ( 'NONE',  ( 0.006176317641841110387, -0.3521105953074989969, 2.465914288053659753 ) ) ;
#12309 = CIRCLE ( 'NONE', #4310, 0.3999999999999999667 ) ;
#12310 = EDGE_CURVE ( 'NONE', #6769, #14398, #16547, .T. ) ;
#12311 = ORIENTED_EDGE ( 'NONE', *, *, #2939, .T. ) ;
#12312 = VECTOR ( 'NONE', #6479, 1000.000000000000000 ) ;
#12313 = PRODUCT_DEFINITION ( 'UNKNOWN', '', #6190, #16593 ) ;
#12314 = CARTESIAN_POINT ( 'NONE',  ( 0.6150581927482109412, -4.451548030288480895, 6.971662190339319665 ) ) ;
#12315 = ADVANCED_FACE ( 'NONE', ( #3566 ), #14877, .T. ) ;
#12316 = DIRECTION ( 'NONE',  ( -1.000000000000000000, 0.000000000000000000, -1.850371707708589879E-16 ) ) ;
#12317 = CARTESIAN_POINT ( 'NONE',  ( -1.899999999999999911, 2.799999999999999822, 0.6099999999999999867 ) ) ;
#12318 = EDGE_CURVE ( 'NONE', #8531, #13986, #5056, .T. ) ;
#12319 = EDGE_CURVE ( 'NONE', #5474, #14839, #13481, .T. ) ;
#12320 = CARTESIAN_POINT ( 'NONE',  ( -0.6343239990445920240, -2.099430913171359769, 2.433641963034089972 ) ) ;
#12321 = DIRECTION ( 'NONE',  ( 3.749399456654639914E-33, 1.000000000000000000, 6.123233995736769734E-17 ) ) ;
#12322 = CARTESIAN_POINT ( 'NONE',  ( 1.810994336139499783, -2.681638120378568857, 5.667058093962681120 ) ) ;
#12323 = VECTOR ( 'NONE', #12084, 1000.000000000000000 ) ;
#12324 = LINE ( 'NONE', #12415, #9404 ) ;
#12325 = CARTESIAN_POINT ( 'NONE',  ( -1.873832970144350130, -0.5625000000000005551, 2.826167029855650270 ) ) ;
#12326 = VERTEX_POINT ( 'NONE', #12002 ) ;
#12327 = FACE_OUTER_BOUND ( 'NONE', #4769, .T. ) ;
#12328 = DIRECTION ( 'NONE',  ( 0.000000000000000000, 0.000000000000000000, -1.000000000000000000 ) ) ;
#12329 = ORIENTED_EDGE ( 'NONE', *, *, #1729, .T. ) ;
#12330 = ORIENTED_EDGE ( 'NONE', *, *, #7501, .T. ) ;
#12331 = VECTOR ( 'NONE', #13048, 1000.000000000000000 ) ;
#12332 = UNCERTAINTY_MEASURE_WITH_UNIT (LENGTH_MEASURE( 1.000000000000000082E-05 ), #9621, 'distance_accuracy_value', 'NONE');
#12333 = ORIENTED_EDGE ( 'NONE', *, *, #15264, .F. ) ;
#12334 = DIRECTION ( 'NONE',  ( 1.903239470785979823E-16, 1.000000000000000000, 0.000000000000000000 ) ) ;
#12335 = CARTESIAN_POINT ( 'NONE',  ( 2.058670345754650022, -5.050847457627120285, 3.559656372813920111 ) ) ;
#12336 = ADVANCED_FACE ( 'NONE', ( #6438 ), #10708, .F. ) ;
#12337 = VECTOR ( 'NONE', #2595, 1000.000000000000000 ) ;
#12338 = CARTESIAN_POINT ( 'NONE',  ( -1.889999999999999902, 7.900000000000000355, 2.126957699879220439E-15 ) ) ;
#12339 = CARTESIAN_POINT ( 'NONE',  ( -0.1749999999999999889, 8.800000000000000711, 0.4000000000000000222 ) ) ;
#12340 = CARTESIAN_POINT ( 'NONE',  ( -2.316126390218390618, -4.734848366107908824, 3.404364157709380390 ) ) ;
#12341 = DIRECTION ( 'NONE',  ( -0.06030856937325100586, -0.9963562379592471041, 0.06030856937324956257 ) ) ;
#12342 = CARTESIAN_POINT ( 'NONE',  ( -1.197297565406129971, -1.517223705964160008, 6.726135293448209929 ) ) ;
#12343 = VECTOR ( 'NONE', #2838, 1000.000000000000000 ) ;
#12344 = CARTESIAN_POINT ( 'NONE',  ( 2.180207327701309872, -0.09343220338983100615, 5.586116916730190063 ) ) ;
#12345 = ORIENTED_EDGE ( 'NONE', *, *, #8601, .T. ) ;
#12346 = CARTESIAN_POINT ( 'NONE',  ( -2.155845792290839835, -0.5447033898305089217, 3.756158857535780271 ) ) ;
#12347 = ORIENTED_EDGE ( 'NONE', *, *, #11770, .T. ) ;
#12348 = VECTOR ( 'NONE', #2542, 1000.000000000000000 ) ;
#12349 = CARTESIAN_POINT ( 'NONE',  ( 2.087380238839969593, -0.1067796610169500227, 6.338810156469096846 ) ) ;
#12350 = VECTOR ( 'NONE', #16452, 1000.000000000000000 ) ;
#12351 = ORIENTED_EDGE ( 'NONE', *, *, #5085, .F. ) ;
#12352 = DIRECTION ( 'NONE',  ( 0.000000000000000000, -1.000000000000000000, 2.775557561562890365E-16 ) ) ;
#12353 = CARTESIAN_POINT ( 'NONE',  ( 1.626408692231650299, -0.8922807985403480302, 6.401040991074950171 ) ) ;
#12354 = CARTESIAN_POINT ( 'NONE',  ( -1.978267656359410154, -5.497669491525420504, 5.974740860598790171 ) ) ;
#12355 = VECTOR ( 'NONE', #10370, 1000.000000000000000 ) ;
#12356 = CARTESIAN_POINT ( 'NONE',  ( -2.471388659209118543, -1.381334852594401363, 5.667135868497515716 ) ) ;
#12357 = EDGE_CURVE ( 'NONE', #10138, #9165, #1079, .T. ) ;
#12358 = ORIENTED_EDGE ( 'NONE', *, *, #108, .F. ) ;
#12359 = LINE ( 'NONE', #16972, #4585 ) ;
#12360 = CARTESIAN_POINT ( 'NONE',  ( 2.036910256464071090, -0.6593979156574641953, 4.443293066459086837 ) ) ;
#12361 = CARTESIAN_POINT ( 'NONE',  ( -0.2908063684825371031, -4.544701183441625325, 7.337905485238597869 ) ) ;
#12362 = CIRCLE ( 'NONE', #1418, 0.5291502622129179434 ) ;
#12363 = CARTESIAN_POINT ( 'NONE',  ( -2.500000000000000000, 11.29999999999999893, 7.649999999999999467 ) ) ;
#12364 = CARTESIAN_POINT ( 'NONE',  ( -1.000000000000000000, -5.599999999999999645, 5.100000000000000533 ) ) ;
#12365 = DIRECTION ( 'NONE',  ( 1.059690869644410208E-14, 1.000000000000000000, -1.041146930477340028E-32 ) ) ;
#12366 = CARTESIAN_POINT ( 'NONE',  ( 0.8014931112107362976, -1.284340823081270733, 6.590108630558003000 ) ) ;
#12367 = CARTESIAN_POINT ( 'NONE',  ( 0.5500000000000000444, 6.450000000000000178, 3.399999999999999911 ) ) ;
#12368 = ORIENTED_EDGE ( 'NONE', *, *, #14430, .T. ) ;
#12369 = CARTESIAN_POINT ( 'NONE',  ( 7.233457020361919865E-16, 4.000000000000000000, 5.100000000000000533 ) ) ;
#12370 = CARTESIAN_POINT ( 'NONE',  ( 1.000000000000000000, -7.000000000000000000, 3.700000000000000178 ) ) ;
#12371 = CARTESIAN_POINT ( 'NONE',  ( 0.5664586606772286093, -0.3133474576271193524, 2.726727161522279452 ) ) ;
#12372 = CIRCLE ( 'NONE', #14717, 0.5999999999999998668 ) ;
#12373 = CARTESIAN_POINT ( 'NONE',  ( -2.339254516529639449, -2.918361879621429011, 5.953396186326395778 ) ) ;
#12374 = CARTESIAN_POINT ( 'NONE',  ( -0.8092638295168710361, -4.911779243796849492, 2.486823565593869745 ) ) ;
#12375 = CARTESIAN_POINT ( 'NONE',  ( -1.088937603231280304, -5.273305084745764759, 2.959627624143549074 ) ) ;
#12376 = VERTEX_POINT ( 'NONE', #16353 ) ;
#12377 = CIRCLE ( 'NONE', #15040, 0.2500000000000002220 ) ;
#12378 = CIRCLE ( 'NONE', #13855, 0.3500000000000001998 ) ;
#12379 = DIRECTION ( 'NONE',  ( -1.000000000000000000, 0.000000000000000000, 7.401486830834370362E-16 ) ) ;
#12380 = CYLINDRICAL_SURFACE ( 'NONE', #14724, 0.5000000000000000000 ) ;
#12381 = FACE_OUTER_BOUND ( 'NONE', #4255, .T. ) ;
#12382 = ORIENTED_EDGE ( 'NONE', *, *, #2565, .F. ) ;
#12383 = CARTESIAN_POINT ( 'NONE',  ( 2.155845792290829621, -5.355296610169490101, 3.756158857535770057 ) ) ;
#12384 = VECTOR ( 'NONE', #12667, 1000.000000000000000 ) ;
#12385 = CIRCLE ( 'NONE', #9711, 0.5999999999999998668 ) ;
#12386 = CARTESIAN_POINT ( 'NONE',  ( -2.306572132003601450, -4.478677194936736328, 6.012569500204175910 ) ) ;
#12387 = CARTESIAN_POINT ( 'NONE',  ( -2.008025181017680794, -3.520016498756949552, 2.964791492240541171 ) ) ;
#12388 = FACE_OUTER_BOUND ( 'NONE', #16172, .T. ) ;
#12389 = CARTESIAN_POINT ( 'NONE',  ( -2.151546283159490258, -4.711560077819619607, 3.746273477677509955 ) ) ;
#12390 = CARTESIAN_POINT ( 'NONE',  ( -0.5999999999999999778, 7.347880794884128857E-17, 7.599999999999999645 ) ) ;
#12391 = CARTESIAN_POINT ( 'NONE',  ( 1.600000000000000089, 1.928341960302230101E-16, 4.000000000000000000 ) ) ;
#12392 = ORIENTED_EDGE ( 'NONE', *, *, #1913, .T. ) ;
#12393 = LINE ( 'NONE', #18290, #5578 ) ;
#12394 = CARTESIAN_POINT ( 'NONE',  ( 1.255262969126039558E-16, -0.3000000000000002665, 2.050000000000001155 ) ) ;
#12395 = VECTOR ( 'NONE', #11000, 1000.000000000000000 ) ;
#12396 = CARTESIAN_POINT ( 'NONE',  ( 2.347833536521260367, -2.541908390648839777, 4.537447324629859224 ) ) ;
#12397 = FACE_OUTER_BOUND ( 'NONE', #7233, .T. ) ;
#12398 = DIRECTION ( 'NONE',  ( 0.7071067811865470176, 4.329780281177469511E-17, -0.7071067811865480168 ) ) ;
#12399 = CARTESIAN_POINT ( 'NONE',  ( 0.3171869470818560743, -5.444279661016954819, 7.334814496515233095 ) ) ;
#12400 = ORIENTED_EDGE ( 'NONE', *, *, #3826, .T. ) ;
#12401 = CARTESIAN_POINT ( 'NONE',  ( 2.500000000000000000, 4.700000000000000178, 1.600000000000000089 ) ) ;
#12402 = CARTESIAN_POINT ( 'NONE',  ( 0.2812789908084389334, -5.144279661016949667, 7.036533610117277959 ) ) ;
#12403 = CARTESIAN_POINT ( 'NONE',  ( -1.550000000000000044, -5.599999999999999645, 6.100000000000000533 ) ) ;
#12404 = DIRECTION ( 'NONE',  ( 0.000000000000000000, 1.000000000000000000, 0.000000000000000000 ) ) ;
#12405 = ORIENTED_EDGE ( 'NONE', *, *, #2230, .T. ) ;
#12406 = CARTESIAN_POINT ( 'NONE',  ( 1.219286470748990103, -4.381683165423610582, 6.712979431025659416 ) ) ;
#12407 = DIRECTION ( 'NONE',  ( 1.850371707708589879E-16, 0.000000000000000000, -1.000000000000000000 ) ) ;
#12408 = DIRECTION ( 'NONE',  ( -1.000000000000000000, 0.000000000000000000, 0.000000000000000000 ) ) ;
#12409 = AXIS2_PLACEMENT_3D ( 'NONE', #7692, #13338, #650 ) ;
#12410 = LINE ( 'NONE', #9623, #18079 ) ;
#12411 = LINE ( 'NONE', #14740, #6694 ) ;
#12412 = CARTESIAN_POINT ( 'NONE',  ( -0.4201920264140019956, -2.122719201459649874, 2.384360920086639801 ) ) ;
#12413 = FACE_OUTER_BOUND ( 'NONE', #3911, .T. ) ;
#12414 = CARTESIAN_POINT ( 'NONE',  ( -0.9123513484652393535, -2.052854336594789331, 2.860838000723768815 ) ) ;
#12415 = CARTESIAN_POINT ( 'NONE',  ( 1.800000000000000044, 11.40000000000000036, 7.649999999999999467 ) ) ;
#12416 = CARTESIAN_POINT ( 'NONE',  ( -0.5999999999999999778, 11.40000000000000036, 7.599999999999999645 ) ) ;
#12417 = EDGE_LOOP ( 'NONE', ( #14007, #14249, #4548, #11512 ) ) ;
#12418 = EDGE_CURVE ( 'NONE', #12787, #12326, #4958, .T. ) ;
#12419 = LINE ( 'NONE', #8258, #15504 ) ;
#12420 = CARTESIAN_POINT ( 'NONE',  ( -0.2564439965878500538, -4.544701183441629766, 7.039440566481220074 ) ) ;
#12421 = ORIENTED_EDGE ( 'NONE', *, *, #7928, .T. ) ;
#12422 = EDGE_CURVE ( 'NONE', #2694, #16856, #3657, .T. ) ;
#12423 = VECTOR ( 'NONE', #12590, 1000.000000000000000 ) ;
#12424 = ORIENTED_EDGE ( 'NONE', *, *, #17579, .F. ) ;
#12425 = EDGE_CURVE ( 'NONE', #4252, #12680, #6724, .T. ) ;
#12426 = VERTEX_POINT ( 'NONE', #902 ) ;
#12427 = CARTESIAN_POINT ( 'NONE',  ( -0.9000000000000000222, 2.050000000000000266, 1.600000000000000089 ) ) ;
#12428 = CARTESIAN_POINT ( 'NONE',  ( -1.057242234132100167, -5.277754237288139194, 2.597442975781530272 ) ) ;
#12429 = LINE ( 'NONE', #13640, #10264 ) ;
#12430 = CARTESIAN_POINT ( 'NONE',  ( 2.350000000000000089, -5.599999999999999645, 2.799999999999999822 ) ) ;
#12431 = DIRECTION ( 'NONE',  ( 0.000000000000000000, -1.000000000000000000, 0.000000000000000000 ) ) ;
#12432 = DIRECTION ( 'NONE',  ( 2.337311630789800155E-16, -1.000000000000000000, -1.168655815394900078E-16 ) ) ;
#12433 = VECTOR ( 'NONE', #11434, 1000.000000000000000 ) ;
#12434 = CARTESIAN_POINT ( 'NONE',  ( 2.151546283159470274, -0.8884399221803740421, 3.746273477677459773 ) ) ;
#12435 = CARTESIAN_POINT ( 'NONE',  ( -2.321479326063761395, -0.2491525423728809807, 3.414080590619972710 ) ) ;
#12436 = EDGE_CURVE ( 'NONE', #1832, #13096, #18000, .T. ) ;
#12437 = PLANE ( 'NONE',  #8794 ) ;
#12438 = ORIENTED_EDGE ( 'NONE', *, *, #14488, .F. ) ;
#12439 = EDGE_CURVE ( 'NONE', #412, #4106, #3938, .T. ) ;
#12440 = CARTESIAN_POINT ( 'NONE',  ( -1.467041701146829746, -0.1779661016949160846, 6.911479965439912831 ) ) ;
#12441 = LINE ( 'NONE', #16785, #957 ) ;
#12442 = EDGE_LOOP ( 'NONE', ( #16786, #7384, #10461, #1955 ) ) ;
#12443 = EDGE_CURVE ( 'NONE', #9752, #16414, #703, .T. ) ;
#12444 = LINE ( 'NONE', #16787, #5870 ) ;
#12445 = CARTESIAN_POINT ( 'NONE',  ( 1.097561405233190568, -1.986830348089889897, 2.618148744692250673 ) ) ;
#12446 = AXIS2_PLACEMENT_3D ( 'NONE', #13856, #11354, #16905 ) ;
#12447 = CARTESIAN_POINT ( 'NONE',  ( 0.06264882350516240428, -5.448728813559320372, 7.052569299041220319 ) ) ;
#12448 = CARTESIAN_POINT ( 'NONE',  ( 2.199635523370541357, -0.5429564742160235546, 3.215170965528963531 ) ) ;
#12449 = EDGE_LOOP ( 'NONE', ( #17180, #452, #1933, #1862 ) ) ;
#12450 = CARTESIAN_POINT ( 'NONE',  ( -0.8001898266890440370, -1.470647129387580021, 6.913242401714570384 ) ) ;
#12451 = CARTESIAN_POINT ( 'NONE',  ( 1.861802609626429961, -0.7991276453871953844, 5.565212624397201324 ) ) ;
#12452 = CARTESIAN_POINT ( 'NONE',  ( -1.008962495263940662, -4.614566048306495638, 7.154609617872592864 ) ) ;
#12453 = DIRECTION ( 'NONE',  ( 1.000000000000000000, -1.224646799147350002E-16, 0.000000000000000000 ) ) ;
#12454 = CARTESIAN_POINT ( 'NONE',  ( -1.000000000000000000, -5.500000000000000000, 5.100000000000000533 ) ) ;
#12455 = CARTESIAN_POINT ( 'NONE',  ( -1.399999999999999911, -7.000000000000000000, 6.100000000000000533 ) ) ;
#12456 = CARTESIAN_POINT ( 'NONE',  ( 1.790316459643169100, -0.8651516338920848259, 3.695177221627173214 ) ) ;
#12457 = DIRECTION ( 'NONE',  ( 1.000000000000000000, 0.000000000000000000, 0.000000000000000000 ) ) ;
#12458 = VERTEX_POINT ( 'NONE', #10798 ) ;
#12459 = CYLINDRICAL_SURFACE ( 'NONE', #11323, 0.6000000000000000888 ) ;
#12460 = DIRECTION ( 'NONE',  ( 0.9622640697945186172, -0.2721173643531222264, 0.000000000000000000 ) ) ;
#12461 = CARTESIAN_POINT ( 'NONE',  ( -1.432215783582709401, -0.1868644067796619845, 6.170863372171116801 ) ) ;
#12462 = ADVANCED_FACE ( 'NONE', ( #16444 ), #3753, .T. ) ;
#12463 = CARTESIAN_POINT ( 'NONE',  ( -0.1366863161730529075, -2.662190708450249854, 7.350364228549148393 ) ) ;
#12464 = CARTESIAN_POINT ( 'NONE',  ( 0.009452110982653640428, -5.000192044704539818, 2.350000000000000089 ) ) ;
#12465 = CARTESIAN_POINT ( 'NONE',  ( 1.134881315981519645, -5.422033898305085309, 6.410767520434657918 ) ) ;
#12466 = VERTEX_POINT ( 'NONE', #4125 ) ;
#12467 = LINE ( 'NONE', #2834, #6831 ) ;
#12468 = CARTESIAN_POINT ( 'NONE',  ( -1.754629622497533634E-17, 5.284133041668071407, 6.863447236587855826 ) ) ;
#12469 = CARTESIAN_POINT ( 'NONE',  ( -1.899999999999999911, 0.7211102550927970256, 7.649999999999999467 ) ) ;
#12470 = ORIENTED_EDGE ( 'NONE', *, *, #2705, .F. ) ;
#12471 = CARTESIAN_POINT ( 'NONE',  ( -2.088297318559229954, -5.502118644067800268, 5.785136623276639689 ) ) ;
#12472 = CARTESIAN_POINT ( 'NONE',  ( -2.185196738168510233, -4.758136654396205145, 3.194002352996703653 ) ) ;
#12473 = CARTESIAN_POINT ( 'NONE',  ( 2.642463257358089734, -4.148800282540726414, 4.945970783863369746 ) ) ;
#12474 = EDGE_CURVE ( 'NONE', #16239, #11906, #12467, .T. ) ;
#12475 = DIRECTION ( 'NONE',  ( -2.854859206178970228E-16, -1.000000000000000000, 0.000000000000000000 ) ) ;
#12476 = CARTESIAN_POINT ( 'NONE',  ( -1.803891155489810050, -4.781424942684489920, 3.188470185434129966 ) ) ;
#12477 = DIRECTION ( 'NONE',  ( 0.000000000000000000, 0.000000000000000000, -1.000000000000000000 ) ) ;
#12478 = ORIENTED_EDGE ( 'NONE', *, *, #4216, .F. ) ;
#12479 = ADVANCED_FACE ( 'NONE', ( #8309 ), #15533, .T. ) ;
#12480 = CARTESIAN_POINT ( 'NONE',  ( 1.661700935665417544, -5.037501140877957084, 3.038299064334577082 ) ) ;
#12481 = CARTESIAN_POINT ( 'NONE',  ( -1.811729841638700211, -0.5580508474576270084, 3.197954009834299782 ) ) ;
#12482 = CARTESIAN_POINT ( 'NONE',  ( 2.301223891756920104, -2.611773255513699876, 5.193066210047949660 ) ) ;
#12483 = PLANE ( 'NONE',  #8365 ) ;
#12484 = DIRECTION ( 'NONE',  ( 0.000000000000000000, 0.000000000000000000, 1.000000000000000000 ) ) ;
#12485 = CARTESIAN_POINT ( 'NONE',  ( -2.560337424259679917, -5.537711864406785978, 4.001768473655595848 ) ) ;
#12486 = VERTEX_POINT ( 'NONE', #4401 ) ;
#12487 = ORIENTED_EDGE ( 'NONE', *, *, #2702, .F. ) ;
#12488 = CARTESIAN_POINT ( 'NONE',  ( -0.4360591020458099987, -5.291101694915249176, 2.387347919655840034 ) ) ;
#12489 = CYLINDRICAL_SURFACE ( 'NONE', #15891, 0.2750000000000000222 ) ;
#12490 = DIRECTION ( 'NONE',  ( -1.000000000000000000, -4.336808689942016947E-15, 1.084202172485504276E-14 ) ) ;
#12491 = VECTOR ( 'NONE', #8338, 1000.000000000000000 ) ;
#12492 = ADVANCED_FACE ( 'NONE', ( #63 ), #12748, .T. ) ;
#12493 = ORIENTED_EDGE ( 'NONE', *, *, #8512, .T. ) ;
#12494 = CARTESIAN_POINT ( 'NONE',  ( 1.869848057046569867, -4.288530012270459935, 6.129130480762009725 ) ) ;
#12495 = PRESENTATION_STYLE_ASSIGNMENT (( #4 ) ) ;
#12496 = VECTOR ( 'NONE', #8140, 1000.000000000000000 ) ;
#12497 = CARTESIAN_POINT ( 'NONE',  ( 1.151392222988870895, -5.028306595106930565, 2.990827770388080342 ) ) ;
#12498 = CARTESIAN_POINT ( 'NONE',  ( -0.5500000000000000444, -2.399999999999999911, 3.600000000000000089 ) ) ;
#12499 = LINE ( 'NONE', #7142, #16173 ) ;
#12500 = CARTESIAN_POINT ( 'NONE',  ( 1.021156010535390068, -3.846052534792979927, 2.579625955254269964 ) ) ;
#12501 = CARTESIAN_POINT ( 'NONE',  ( 0.5921572875253799939, 6.450000000000000178, 1.600000000000000089 ) ) ;
#12502 = CARTESIAN_POINT ( 'NONE',  ( -1.279347147864589251, -3.566593075333521767, 3.094331068408299412 ) ) ;
#12503 = DIRECTION ( 'NONE',  ( 1.000000000000000000, -2.220446049250310320E-15, 0.000000000000000000 ) ) ;
#12504 = CARTESIAN_POINT ( 'NONE',  ( 0.8570167067220200163, -0.3177966101694920664, 2.508190348879349774 ) ) ;
#12505 = ORIENTED_EDGE ( 'NONE', *, *, #2983, .T. ) ;
#12506 = VECTOR ( 'NONE', #7979, 1000.000000000000000 ) ;
#12507 = CARTESIAN_POINT ( 'NONE',  ( -0.8934014991059870958, -4.614566048306490309, 6.877287176483410924 ) ) ;
#12508 = VERTEX_POINT ( 'NONE', #5517 ) ;
#12509 = ORIENTED_EDGE ( 'NONE', *, *, #15046, .F. ) ;
#12510 = ADVANCED_FACE ( 'NONE', ( #2555 ), #15352, .F. ) ;
#12511 = UNCERTAINTY_MEASURE_WITH_UNIT (LENGTH_MEASURE( 1.000000000000000082E-05 ), #2497, 'distance_accuracy_value', 'NONE');
#12512 = ORIENTED_EDGE ( 'NONE', *, *, #17102, .F. ) ;
#12513 = DIRECTION ( 'NONE',  ( 0.000000000000000000, 0.000000000000000000, -1.000000000000000000 ) ) ;
#12514 = CARTESIAN_POINT ( 'NONE',  ( 1.494593880360790550, -5.038983050847454237, 3.295456077495951153 ) ) ;
#12515 = DIRECTION ( 'NONE',  ( -1.000000000000000000, -8.881784197001258979E-17, -1.776356839400249824E-16 ) ) ;
#12516 = FACE_OUTER_BOUND ( 'NONE', #17196, .T. ) ;
#12517 = PLANE ( 'NONE',  #14964 ) ;
#12518 = DIRECTION ( 'NONE',  ( 0.000000000000000000, -1.387778780781449866E-16, -1.000000000000000000 ) ) ;
#12519 = ADVANCED_FACE ( 'NONE', ( #18274 ), #1348, .T. ) ;
#12520 = CARTESIAN_POINT ( 'NONE',  ( 1.794646911016580137, -1.167899381639829981, 6.222494056560660347 ) ) ;
#12521 = CARTESIAN_POINT ( 'NONE',  ( 2.270487904532159984, -0.06228813559322070315, 4.080813552109670894 ) ) ;
#12522 = ORIENTED_EDGE ( 'NONE', *, *, #9762, .T. ) ;
#12523 = CARTESIAN_POINT ( 'NONE',  ( 2.270487904532159984, -0.3622881355932209835, 4.080813552109670894 ) ) ;
#12524 = CARTESIAN_POINT ( 'NONE',  ( 1.707817112497189926, -0.4112288135593229477, 6.319218296629480314 ) ) ;
#12525 = EDGE_LOOP ( 'NONE', ( #13203, #5522 ) ) ;
#12526 = CARTESIAN_POINT ( 'NONE',  ( 0.9222751404130974384, -0.02224576271186471527, 2.865854510788131027 ) ) ;
#12527 = DIRECTION ( 'NONE',  ( 1.000000000000000000, 0.000000000000000000, 0.000000000000000000 ) ) ;
#12528 = VERTEX_POINT ( 'NONE', #9874 ) ;
#12529 = DIRECTION ( 'NONE',  ( 0.000000000000000000, 0.000000000000000000, 1.000000000000000000 ) ) ;
#12530 = CARTESIAN_POINT ( 'NONE',  ( 2.349464193210359930, -2.243001519261069721, 4.563019372514570016 ) ) ;
#12531 = CARTESIAN_POINT ( 'NONE',  ( 0.000000000000000000, 0.000000000000000000, 0.000000000000000000 ) ) ;
#12532 = CARTESIAN_POINT ( 'NONE',  ( 2.625437065641401446, -5.381991525423726053, 5.087214675345139270 ) ) ;
#12533 =( REPRESENTATION_RELATIONSHIP ('NONE','NONE', #2757, #16004 ) REPRESENTATION_RELATIONSHIP_WITH_TRANSFORMATION ( #10383 )SHAPE_REPRESENTATION_RELATIONSHIP( ) );
#12534 = ORIENTED_EDGE ( 'NONE', *, *, #16868, .F. ) ;
#12535 = ADVANCED_FACE ( 'NONE', ( #11163 ), #2656, .T. ) ;
#12536 = CARTESIAN_POINT ( 'NONE',  ( -1.981271652668300298, -1.633665147405599871, 5.970160748022450115 ) ) ;
#12537 = CARTESIAN_POINT ( 'NONE',  ( -2.351212046067109984, -4.618406924666470736, 4.597298481426070893 ) ) ;
#12538 = EDGE_CURVE ( 'NONE', #14665, #12508, #8127, .T. ) ;
#12539 = ORIENTED_EDGE ( 'NONE', *, *, #5876, .T. ) ;
#12540 = ADVANCED_FACE ( 'NONE', ( #14654 ), #8747, .T. ) ;
#12541 = CARTESIAN_POINT ( 'NONE',  ( 0.1749999999999999889, 7.700000000000000178, 0.5999999999999999778 ) ) ;
#12542 = CARTESIAN_POINT ( 'NONE',  ( -2.500000000000000000, 11.15000000000000036, 1.600000000000000089 ) ) ;
#12543 = VECTOR ( 'NONE', #17279, 1000.000000000000000 ) ;
#12544 = EDGE_CURVE ( 'NONE', #8588, #12303, #14395, .T. ) ;
#12545 = CARTESIAN_POINT ( 'NONE',  ( 0.9742769543504904428, -1.261052534792989288, 6.507120986223561054 ) ) ;
#12546 = ADVANCED_FACE ( 'NONE', ( #5970 ), #13102, .T. ) ;
#12547 = CARTESIAN_POINT ( 'NONE',  ( 1.875000000000000000, 11.25000000000000000, 8.300000000000000711 ) ) ;
#12548 = ORIENTED_EDGE ( 'NONE', *, *, #15036, .T. ) ;
#12549 = PLANE ( 'NONE',  #968 ) ;
#12550 = CARTESIAN_POINT ( 'NONE',  ( 2.500000000000000000, 0.8000000000000000444, -1.674850734291659957E-15 ) ) ;
#12551 = CARTESIAN_POINT ( 'NONE',  ( 1.246151616534670215, -0.3311440677966111523, 3.068501529594759081 ) ) ;
#12552 = CARTESIAN_POINT ( 'NONE',  ( 1.351547610267151533, -4.082776294035843634, 6.983951126925231456 ) ) ;
#12553 = CARTESIAN_POINT ( 'NONE',  ( -1.074005996636800075, -5.164643153926310681, 2.934052701886380010 ) ) ;
#12554 = CARTESIAN_POINT ( 'NONE',  ( 0.9707742057416334225, -5.126483050847465250, 6.508944043303927174 ) ) ;
#12555 = ORIENTED_EDGE ( 'NONE', *, *, #5910, .T. ) ;
#12556 = CARTESIAN_POINT ( 'NONE',  ( 2.203023580853991081, -0.05783898305084791275, 3.872235369154280349 ) ) ;
#12557 = CARTESIAN_POINT ( 'NONE',  ( -1.408343819019460219E-16, 7.000000000000000000, 5.100000000000000533 ) ) ;
#12558 = CARTESIAN_POINT ( 'NONE',  ( 2.241103642439659443E-15, 9.099999999999999645, 8.300000000000000711 ) ) ;
#12559 = EDGE_LOOP ( 'NONE', ( #15334, #10235, #13756, #17824 ) ) ;
#12560 = CARTESIAN_POINT ( 'NONE',  ( -0.07299321914061848715, -5.598516949152539723, 2.350000000000000089 ) ) ;
#12561 = CARTESIAN_POINT ( 'NONE',  ( 2.239137794397009884, -0.6128213390808879835, 3.975425900939169921 ) ) ;
#12562 = EDGE_CURVE ( 'NONE', #9265, #16145, #7459, .T. ) ;
#12563 = LINE ( 'NONE', #8403, #9072 ) ;
#12564 = CARTESIAN_POINT ( 'NONE',  ( 1.953802435660499048, -0.6128213390808875394, 4.069478085300975323 ) ) ;
#12565 = LINE ( 'NONE', #11174, #3434 ) ;
#12566 = ORIENTED_EDGE ( 'NONE', *, *, #8135, .T. ) ;
#12567 = CARTESIAN_POINT ( 'NONE',  ( 1.738765645129589865, -5.293166154074419261, 2.961234354870410090 ) ) ;
#12568 = CARTESIAN_POINT ( 'NONE',  ( -1.713314936023349944, -0.5610169491525430763, 3.089913064446579760 ) ) ;
#12569 = CARTESIAN_POINT ( 'NONE',  ( -2.295719155670160383, -3.287133615874060055, 5.218091927917240191 ) ) ;
#12570 = CYLINDRICAL_SURFACE ( 'NONE', #3056, 0.1499999999999999667 ) ;
#12571 = DIRECTION ( 'NONE',  ( 1.110223024625159992E-16, 0.000000000000000000, 1.000000000000000000 ) ) ;
#12572 = CARTESIAN_POINT ( 'NONE',  ( 2.650076489488250697, -5.077542372881359789, 4.841243018609314497 ) ) ;
#12573 = ORIENTED_EDGE ( 'NONE', *, *, #15769, .F. ) ;
#12574 = VERTEX_POINT ( 'NONE', #416 ) ;
#12575 = FACE_OUTER_BOUND ( 'NONE', #5568, .T. ) ;
#12576 = DIRECTION ( 'NONE',  ( 0.000000000000000000, 1.233581138472399909E-16, -1.000000000000000000 ) ) ;
#12577 = DIRECTION ( 'NONE',  ( -2.261565420532729920E-16, -1.000000000000000000, 0.000000000000000000 ) ) ;
#12578 = ORIENTED_EDGE ( 'NONE', *, *, #3574, .F. ) ;
#12579 = CARTESIAN_POINT ( 'NONE',  ( -0.2620510901103649815, -3.706322805063249959, 2.361180871966390260 ) ) ;
#12580 = EDGE_CURVE ( 'NONE', #9757, #3082, #6054, .T. ) ;
#12581 = LINE ( 'NONE', #11198, #13242 ) ;
#12582 = CARTESIAN_POINT ( 'NONE',  ( 1.338894208872951186, -5.333856471232010676, 3.139702328019969180 ) ) ;
#12583 = DIRECTION ( 'NONE',  ( -0.2721173643531200059, 0.9622640697945191723, 0.000000000000000000 ) ) ;
#12584 = DIRECTION ( 'NONE',  ( -1.000000000000000000, 0.000000000000000000, 0.000000000000000000 ) ) ;
#12585 = CARTESIAN_POINT ( 'NONE',  ( 2.100188519621589922, -4.009070552810999999, 3.637948273607370275 ) ) ;
#12586 = CARTESIAN_POINT ( 'NONE',  ( -1.699999999999999956, 2.299999999999999822, 7.700000000000000178 ) ) ;
#12587 = CARTESIAN_POINT ( 'NONE',  ( -0.03895741673419786388, -3.729611093351542284, 2.647347042895590086 ) ) ;
#12588 = DIRECTION ( 'NONE',  ( 0.000000000000000000, 1.000000000000000000, 0.000000000000000000 ) ) ;
#12589 = ORIENTED_EDGE ( 'NONE', *, *, #12760, .F. ) ;
#12590 = DIRECTION ( 'NONE',  ( 1.110223024625159992E-16, 0.000000000000000000, 1.000000000000000000 ) ) ;
#12591 = ORIENTED_EDGE ( 'NONE', *, *, #8017, .T. ) ;
#12592 =( NAMED_UNIT ( * ) PLANE_ANGLE_UNIT ( ) SI_UNIT ( $, .RADIAN. ) );
#12593 = ORIENTED_EDGE ( 'NONE', *, *, #8924, .T. ) ;
#12594 = ORIENTED_EDGE ( 'NONE', *, *, #653, .T. ) ;
#12595 = ORIENTED_EDGE ( 'NONE', *, *, #14476, .T. ) ;
#12596 = CARTESIAN_POINT ( 'NONE',  ( -1.899999999999999911, 11.29999999999999893, 7.649999999999999467 ) ) ;
#12597 = ADVANCED_FACE ( 'NONE', ( #17334 ), #4664, .F. ) ;
#12598 = CARTESIAN_POINT ( 'NONE',  ( -2.022304719220918479, -5.233262711864406391, 4.346496488058700258 ) ) ;
#12599 = PRODUCT ( 'MAS-687', 'MAS-687', '', ( #8559 ) ) ;
#12600 = CARTESIAN_POINT ( 'NONE',  ( -2.642175029090489513, -1.497776294035840561, 4.450952196049505538 ) ) ;
#12601 = AXIS2_PLACEMENT_3D ( 'NONE', #2798, #18225, #27 ) ;
#12602 = CYLINDRICAL_SURFACE ( 'NONE', #1982, 0.2000000000000000389 ) ;
#12603 = CARTESIAN_POINT ( 'NONE',  ( -0.9000000000000000222, 6.450000000000000178, 3.600000000000000089 ) ) ;
#12604 = DIRECTION ( 'NONE',  ( -1.168655815394900078E-16, 1.000000000000000000, 0.000000000000000000 ) ) ;
#12605 = DIRECTION ( 'NONE',  ( -1.000000000000000000, 1.224646799147350002E-16, 0.000000000000000000 ) ) ;
#12606 = AXIS2_PLACEMENT_3D ( 'NONE', #3694, #16481, #16583 ) ;
#12607 = VECTOR ( 'NONE', #6608, 1000.000000000000000 ) ;
#12608 = DIRECTION ( 'NONE',  ( -3.392348130799090196E-16, 1.000000000000000000, 0.000000000000000000 ) ) ;
#12609 = CARTESIAN_POINT ( 'NONE',  ( -1.588913656382020756, -5.080331814072260421, 3.399901838171254020 ) ) ;
#12610 = CARTESIAN_POINT ( 'NONE',  ( -1.019987577504920528, -2.778632149891700376, 6.481720287913836920 ) ) ;
#12611 = CARTESIAN_POINT ( 'NONE',  ( -2.043308330018790198, -0.2002118644067800157, 5.867646457774669422 ) ) ;
#12612 = CARTESIAN_POINT ( 'NONE',  ( 2.500000000000000000, 9.199999999999999289, 0.6099999999999999867 ) ) ;
#12613 = CARTESIAN_POINT ( 'NONE',  ( 0.6500000000000000222, 6.450000000000000178, 3.200000000000000178 ) ) ;
#12614 = ORIENTED_EDGE ( 'NONE', *, *, #6297, .F. ) ;
#12615 = CARTESIAN_POINT ( 'NONE',  ( 2.353194804772640314, -0.07563559322033940047, 4.731327187377229571 ) ) ;
#12616 = CARTESIAN_POINT ( 'NONE',  ( 0.4985810152601650724, -1.330917399657850053, 7.000035360316460675 ) ) ;
#12617 = ORIENTED_EDGE ( 'NONE', *, *, #9794, .F. ) ;
#12618 = CARTESIAN_POINT ( 'NONE',  ( 1.300000000000000044, -1.592040838891560081E-16, 7.700000000000000178 ) ) ;
#12619 = AXIS2_PLACEMENT_3D ( 'NONE', #3486, #16181, #9427 ) ;
#12620 = ORIENTED_EDGE ( 'NONE', *, *, #6390, .F. ) ;
#12621 = CARTESIAN_POINT ( 'NONE',  ( -2.337178851518210365, -3.011515032774579659, 4.976298214796807784 ) ) ;
#12622 = CARTESIAN_POINT ( 'NONE',  ( -0.8570167067220350043, -5.582203389830509899, 2.508190348879359988 ) ) ;
#12623 = AXIS2_PLACEMENT_3D ( 'NONE', #14904, #8968, #14703 ) ;
#12624 = VERTEX_POINT ( 'NONE', #10400 ) ;
#12625 = CARTESIAN_POINT ( 'NONE',  ( 2.231116159141619981, -0.9117282104686620370, 3.951089877392439664 ) ) ;
#12626 = CARTESIAN_POINT ( 'NONE',  ( 1.489797906646480596, -0.4112288135593234473, 6.112509577910826941 ) ) ;
#12627 = VECTOR ( 'NONE', #7377, 1000.000000000000000 ) ;
#12628 = VERTEX_POINT ( 'NONE', #16061 ) ;
#12629 = PLANE ( 'NONE',  #5814 ) ;
#12630 = CARTESIAN_POINT ( 'NONE',  ( 5.829811056852225605E-17, 3.957026083511936854, 8.102080397533582001 ) ) ;
#12631 = CARTESIAN_POINT ( 'NONE',  ( -2.616666666666669805, -4.318079751576579732E-16, 4.000000000000000000 ) ) ;
#12632 = CARTESIAN_POINT ( 'NONE',  ( 1.572563554680340703, -0.8185750573155082810, 3.380172092915559645 ) ) ;
#12633 = CARTESIAN_POINT ( 'NONE',  ( 0.1749999999999999889, 9.099999999999999645, 0.5999999999999999778 ) ) ;
#12634 = CARTESIAN_POINT ( 'NONE',  ( 1.747582379783020778, -0.4156779661016956062, 6.697200745122486865 ) ) ;
#12635 = AXIS2_PLACEMENT_3D ( 'NONE', #1089, #6737, #13691 ) ;
#12636 = ORIENTED_EDGE ( 'NONE', *, *, #12474, .T. ) ;
#12637 = FACE_OUTER_BOUND ( 'NONE', #13684, .T. ) ;
#12638 = VECTOR ( 'NONE', #11490, 1000.000000000000000 ) ;
#12639 = DIRECTION ( 'NONE',  ( 6.123233995736769734E-17, -1.368455531567203867E-48, 1.000000000000000000 ) ) ;
#12640 = CARTESIAN_POINT ( 'NONE',  ( -1.940327948426050941, -0.2091101694915259990, 5.370677689277675526 ) ) ;
#12641 = VECTOR ( 'NONE', #4470, 1000.000000000000000 ) ;
#12642 = CARTESIAN_POINT ( 'NONE',  ( 1.558664967382918931, -4.059488005747546424, 6.847947208954417775 ) ) ;
#12643 = AXIS2_PLACEMENT_3D ( 'NONE', #10859, #10954, #12341 ) ;
#12644 = CIRCLE ( 'NONE', #1122, 0.4166666666666670737 ) ;
#12645 = CARTESIAN_POINT ( 'NONE',  ( -1.695999708020951013, -5.128627060139315574, 2.646274854235481921 ) ) ;
#12646 = CARTESIAN_POINT ( 'NONE',  ( -1.351903350398179438, -5.184322033898315141, 6.245004350000422200 ) ) ;
#12647 = EDGE_LOOP ( 'NONE', ( #9067, #11686, #12237, #5623 ) ) ;
#12648 = EDGE_CURVE ( 'NONE', #7773, #9755, #1968, .T. ) ;
#12649 = VECTOR ( 'NONE', #5765, 1000.000000000000000 ) ;
#12650 = CARTESIAN_POINT ( 'NONE',  ( 1.851073041990159540, -0.1067796610169499810, 6.153284478378259870 ) ) ;
#12651 = ADVANCED_FACE ( 'NONE', ( #9091 ), #9478, .T. ) ;
#12652 = CARTESIAN_POINT ( 'NONE',  ( 1.811729841638690219, -5.341949152542369461, 3.197954009834290012 ) ) ;
#12653 = LINE ( 'NONE', #5711, #5239 ) ;
#12654 = EDGE_CURVE ( 'NONE', #2568, #8419, #678, .T. ) ;
#12655 = ORIENTED_EDGE ( 'NONE', *, *, #1806, .F. ) ;
#12656 = VECTOR ( 'NONE', #9772, 1000.000000000000000 ) ;
#12657 = LINE ( 'NONE', #18278, #16471 ) ;
#12658 = CIRCLE ( 'NONE', #15619, 0.4166666666666669072 ) ;
#12659 = CARTESIAN_POINT ( 'NONE',  ( -2.353452300571019506, -1.474488005747550012, 4.697179287168410156 ) ) ;
#12660 = DIRECTION ( 'NONE',  ( 0.000000000000000000, 0.000000000000000000, 1.000000000000000000 ) ) ;
#12661 = CARTESIAN_POINT ( 'NONE',  ( -2.043688444617268729, -1.497776294035840561, 4.504451070148879133 ) ) ;
#12662 = VECTOR ( 'NONE', #16012, 1000.000000000000000 ) ;
#12663 = VECTOR ( 'NONE', #12577, 1000.000000000000000 ) ;
#12664 = CARTESIAN_POINT ( 'NONE',  ( 1.149999999999999911, 9.274118095489749081, 7.596592582628910684 ) ) ;
#12665 = EDGE_LOOP ( 'NONE', ( #18138, #6727, #13009, #17754 ) ) ;
#12666 = CIRCLE ( 'NONE', #7343, 0.3999999999999999667 ) ;
#12667 = DIRECTION ( 'NONE',  ( -1.903239470785979823E-16, -1.000000000000000000, 0.000000000000000000 ) ) ;
#12668 = CARTESIAN_POINT ( 'NONE',  ( 2.386628511786341722, -0.3533898305084745561, 3.539457309197775459 ) ) ;
#12669 = CARTESIAN_POINT ( 'NONE',  ( -2.237394498046660019, -3.263845327585780165, 5.429939413646380331 ) ) ;
#12670 = CYLINDRICAL_SURFACE ( 'NONE', #5717, 0.2499999999999996669 ) ;
#12671 = CARTESIAN_POINT ( 'NONE',  ( 0.000000000000000000, 3.050000000000000266, 1.867586368699710122E-16 ) ) ;
#12672 = CARTESIAN_POINT ( 'NONE',  ( 2.020286629067969297, -5.108686440677975504, 6.420841923842827370 ) ) ;
#12673 = ORIENTED_EDGE ( 'NONE', *, *, #7007, .F. ) ;
#12674 = EDGE_CURVE ( 'NONE', #6214, #9105, #3541, .T. ) ;
#12675 = VERTEX_POINT ( 'NONE', #9382 ) ;
#12676 = CARTESIAN_POINT ( 'NONE',  ( 0.6628679656440349399, 6.450000000000000178, 1.670710678118660031 ) ) ;
#12677 = AXIS2_PLACEMENT_3D ( 'NONE', #9699, #14145, #15545 ) ;
#12678 = CARTESIAN_POINT ( 'NONE',  ( 4.265698758777729940E-16, 2.350000000000000089, 8.300000000000000711 ) ) ;
#12679 = AXIS2_PLACEMENT_3D ( 'NONE', #6847, #2500, #15191 ) ;
#12680 = VERTEX_POINT ( 'NONE', #4838 ) ;
#12681 = CARTESIAN_POINT ( 'NONE',  ( 0.06913820924143311564, -1.377493976234431372, 7.352985789827153340 ) ) ;
#12682 = AXIS2_PLACEMENT_3D ( 'NONE', #2633, #15227, #16694 ) ;
#12683 = CARTESIAN_POINT ( 'NONE',  ( 1.097896950867359500, -0.7068739681193977331, 2.280088753565270743 ) ) ;
#12684 = CARTESIAN_POINT ( 'NONE',  ( 0.5677251586959709551, -5.311531839079339790, 2.399563163165729929 ) ) ;
#12685 = DIRECTION ( 'NONE',  ( -1.708035422500239940E-16, -1.000000000000000000, -8.540177112501199701E-17 ) ) ;
#12686 = CARTESIAN_POINT ( 'NONE',  ( -1.923406176634930853, -4.796950468210009255, 2.875176962145308934 ) ) ;
#12687 = DIRECTION ( 'NONE',  ( 0.000000000000000000, 0.000000000000000000, -1.000000000000000000 ) ) ;
#12688 = CARTESIAN_POINT ( 'NONE',  ( 1.401708661791409849, -4.358394877135329359, 6.590491606684049763 ) ) ;
#12689 = VECTOR ( 'NONE', #16010, 1000.000000000000000 ) ;
#12690 = CARTESIAN_POINT ( 'NONE',  ( -0.9000000000000000222, -9.500000000000000000, 6.100000000000000533 ) ) ;
#12691 = VECTOR ( 'NONE', #11496, 1000.000000000000000 ) ;
#12692 = CARTESIAN_POINT ( 'NONE',  ( 1.058024172752470182, -3.869340823081269587, 2.940600473883339561 ) ) ;
#12693 = DIRECTION ( 'NONE',  ( -2.337311630789800155E-16, 1.000000000000000000, 0.000000000000000000 ) ) ;
#12694 = CARTESIAN_POINT ( 'NONE',  ( 1.289999999999999813, 7.900000000000003908, 0.6000000000000025313 ) ) ;
#12695 = ORIENTED_EDGE ( 'NONE', *, *, #5458, .F. ) ;
#12696 = LINE ( 'NONE', #6859, #14757 ) ;
#12697 = ORIENTED_EDGE ( 'NONE', *, *, #9352, .F. ) ;
#12698 = EDGE_CURVE ( 'NONE', #18021, #2376, #10684, .T. ) ;
#12699 =( GEOMETRIC_REPRESENTATION_CONTEXT ( 3 ) GLOBAL_UNCERTAINTY_ASSIGNED_CONTEXT ( ( #10847 ) ) GLOBAL_UNIT_ASSIGNED_CONTEXT ( ( #5546, #14154, #9709 ) ) REPRESENTATION_CONTEXT ( 'NONE', 'WORKASPACE' ) );
#12700 = CARTESIAN_POINT ( 'NONE',  ( 1.289999999999999813, 4.099999999999999645, 6.203059698991501599E-15 ) ) ;
#12701 = ORIENTED_EDGE ( 'NONE', *, *, #7660, .T. ) ;
#12702 = PLANE ( 'NONE',  #3496 ) ;
#12703 = UNCERTAINTY_MEASURE_WITH_UNIT (LENGTH_MEASURE( 1.000000000000000082E-05 ), #9480, 'distance_accuracy_value', 'NONE');
#12704 = ORIENTED_EDGE ( 'NONE', *, *, #15794, .F. ) ;
#12705 = AXIS2_PLACEMENT_3D ( 'NONE', #13745, #1251, #15338 ) ;
#12706 = CARTESIAN_POINT ( 'NONE',  ( -2.052786957354850728, -5.224364406779660186, 4.727327971967373976 ) ) ;
#12707 = CARTESIAN_POINT ( 'NONE',  ( -2.549960444629829848, -1.544352870612421880, 3.964598460822165382 ) ) ;
#12708 = DIRECTION ( 'NONE',  ( 0.000000000000000000, 0.000000000000000000, 1.000000000000000000 ) ) ;
#12709 = CARTESIAN_POINT ( 'NONE',  ( 1.399999999999999911, -8.000000000000000000, 3.299999999999999822 ) ) ;
#12710 = LINE ( 'NONE', #8271, #6757 ) ;
#12711 = DIRECTION ( 'NONE',  ( 1.930822651522009842E-16, 1.000000000000000000, -1.268826313857319964E-16 ) ) ;
#12712 = PRODUCT_DEFINITION_FORMATION_WITH_SPECIFIED_SOURCE ( 'ANY', '', #13935, .NOT_KNOWN. ) ;
#12713 = CYLINDRICAL_SURFACE ( 'NONE', #17377, 0.5000000000000000000 ) ;
#12714 = CARTESIAN_POINT ( 'NONE',  ( 0.5570002967656469961, -2.891232714973159812, 6.986590552960210587 ) ) ;
#12715 = CARTESIAN_POINT ( 'NONE',  ( 1.583713126240741564, -2.429307825567371459, 6.006428174987391344 ) ) ;
#12716 = CARTESIAN_POINT ( 'NONE',  ( 1.901882987994760965, -0.09343220338983100615, 5.472995608211450147 ) ) ;
#12717 = LINE ( 'NONE', #11324, #14426 ) ;
#12718 = VECTOR ( 'NONE', #1097, 1000.000000000000000 ) ;
#12719 = FACE_OUTER_BOUND ( 'NONE', #6051, .T. ) ;
#12720 = VERTEX_POINT ( 'NONE', #16141 ) ;
#12721 = EDGE_CURVE ( 'NONE', #11001, #17501, #3268, .T. ) ;
#12722 = CARTESIAN_POINT ( 'NONE',  ( -2.328217775191430139, -0.2180084745762720100, 5.043379051721170292 ) ) ;
#12723 = CARTESIAN_POINT ( 'NONE',  ( 2.023259452208809872, -2.425466949207399914, 3.497849062500220096 ) ) ;
#12724 = ORIENTED_EDGE ( 'NONE', *, *, #13902, .T. ) ;
#12725 = VERTEX_POINT ( 'NONE', #7607 ) ;
#12726 = CARTESIAN_POINT ( 'NONE',  ( 2.334032080503399609, -2.289578095837639715, 5.001728246382188381 ) ) ;
#12727 = DIRECTION ( 'NONE',  ( 0.000000000000000000, 0.000000000000000000, 1.000000000000000000 ) ) ;
#12728 = CARTESIAN_POINT ( 'NONE',  ( -0.6493550500446439999, -5.586652542372879005, 2.437955526623099889 ) ) ;
#12729 = ORIENTED_EDGE ( 'NONE', *, *, #10487, .F. ) ;
#12730 = FACE_OUTER_BOUND ( 'NONE', #17252, .T. ) ;
#12731 = VECTOR ( 'NONE', #11279, 1000.000000000000000 ) ;
#12732 = CARTESIAN_POINT ( 'NONE',  ( -0.6187874668174415671, -0.4646186440677965712, 6.657494107589526422 ) ) ;
#12733 = ORIENTED_EDGE ( 'NONE', *, *, #13199, .T. ) ;
#12734 = FACE_OUTER_BOUND ( 'NONE', #16515, .T. ) ;
#12735 = CARTESIAN_POINT ( 'NONE',  ( -1.385380178477320312, -1.982989471729918352, 3.184868453331453075 ) ) ;
#12736 = CARTESIAN_POINT ( 'NONE',  ( 0.4000000000000000222, 2.399999999999999911, 5.100000000000000533 ) ) ;
#12737 = CARTESIAN_POINT ( 'NONE',  ( 1.610878918935058524, -0.3311440677966099311, 2.590989782159081933 ) ) ;
#12738 = ORIENTED_EDGE ( 'NONE', *, *, #3686, .T. ) ;
#12739 = DIRECTION ( 'NONE',  ( 0.000000000000000000, -1.000000000000000000, -1.110223024625160090E-15 ) ) ;
#12740 = EDGE_CURVE ( 'NONE', #7150, #17150, #15125, .T. ) ;
#12741 = CARTESIAN_POINT ( 'NONE',  ( -2.500000000000000000, 9.199999999999999289, 0.6099999999999999867 ) ) ;
#12742 = CARTESIAN_POINT ( 'NONE',  ( -0.6187874668174415671, -0.4646186440677965712, 6.657494107589526422 ) ) ;
#12743 = VERTEX_POINT ( 'NONE', #7992 ) ;
#12744 = VECTOR ( 'NONE', #14975, 1000.000000000000000 ) ;
#12745 = CARTESIAN_POINT ( 'NONE',  ( -1.209303714320900003, -4.865515740159329638, 2.662663894020049771 ) ) ;
#12746 = CARTESIAN_POINT ( 'NONE',  ( -0.1365430262726299304, -5.453177966101685037, 6.748423079423377047 ) ) ;
#12747 = VERTEX_POINT ( 'NONE', #16219 ) ;
#12748 = PLANE ( 'NONE',  #10085 ) ;
#12749 = DIRECTION ( 'NONE',  ( 1.000000000000000000, 0.000000000000000000, 0.000000000000000000 ) ) ;
#12750 = DIRECTION ( 'NONE',  ( 1.000000000000000000, 0.000000000000000000, 0.000000000000000000 ) ) ;
#12751 = ORIENTED_EDGE ( 'NONE', *, *, #8937, .F. ) ;
#12752 = DIRECTION ( 'NONE',  ( -1.000000000000000000, 0.000000000000000000, 0.000000000000000000 ) ) ;
#12753 = CARTESIAN_POINT ( 'NONE',  ( 2.033393610350129777, -0.8224159336754830463, 5.884928737465320303 ) ) ;
#12754 = FACE_OUTER_BOUND ( 'NONE', #12031, .T. ) ;
#12755 = VECTOR ( 'NONE', #9829, 1000.000000000000000 ) ;
#12756 = CARTESIAN_POINT ( 'NONE',  ( -1.333132471082830506, -2.825208726468270370, 6.261300629978947541 ) ) ;
#12757 = ADVANCED_FACE ( 'NONE', ( #7884 ), #4814, .T. ) ;
#12758 = CARTESIAN_POINT ( 'NONE',  ( -1.599999999999880185, 11.40000000000000036, -2.399999999999999911 ) ) ;
#12759 = VERTEX_POINT ( 'NONE', #12241 ) ;
#12760 = EDGE_CURVE ( 'NONE', #14294, #12466, #7718, .T. ) ;
#12761 = CYLINDRICAL_SURFACE ( 'NONE', #16803, 0.1999999999999999833 ) ;
#12762 = CARTESIAN_POINT ( 'NONE',  ( 2.653602652190420574, -0.07563559322033948373, 4.735326402787084277 ) ) ;
#12763 = CARTESIAN_POINT ( 'NONE',  ( -1.465095039565370127, -3.566593075333519991, 2.858195935359880480 ) ) ;
#12764 = DIRECTION ( 'NONE',  ( 3.007035789127644200E-16, 1.000000000000000000, -1.202814315651057680E-15 ) ) ;
#12765 = DIRECTION ( 'NONE',  ( 0.000000000000000000, 0.000000000000000000, 1.000000000000000000 ) ) ;
#12766 = CARTESIAN_POINT ( 'NONE',  ( -1.407651048079459288, -5.573305084745765470, 2.450250343405070641 ) ) ;
#12767 = ORIENTED_EDGE ( 'NONE', *, *, #13367, .T. ) ;
#12768 = ORIENTED_EDGE ( 'NONE', *, *, #5419, .T. ) ;
#12769 = FACE_OUTER_BOUND ( 'NONE', #8287, .T. ) ;
#12770 = LINE ( 'NONE', #4235, #13849 ) ;
#12771 = ORIENTED_EDGE ( 'NONE', *, *, #9715, .F. ) ;
#12772 = CARTESIAN_POINT ( 'NONE',  ( 2.626509418457480649, -1.028169651910100679, 5.080213055741780614 ) ) ;
#12773 = ADVANCED_FACE ( 'NONE', ( #576 ), #3527, .T. ) ;
#12774 =( NAMED_UNIT ( * ) PLANE_ANGLE_UNIT ( ) SI_UNIT ( $, .RADIAN. ) );
#12775 = CARTESIAN_POINT ( 'NONE',  ( -1.500000000000000000, -6.000000000000000000, 2.299999999999999822 ) ) ;
#12776 = LINE ( 'NONE', #11016, #1217 ) ;
#12777 = CARTESIAN_POINT ( 'NONE',  ( -2.510208264418979596, -4.525253771513313872, 5.561375738133230939 ) ) ;
#12778 = EDGE_CURVE ( 'NONE', #2630, #13454, #16313, .T. ) ;
#12779 = EDGE_CURVE ( 'NONE', #16312, #5150, #7701, .T. ) ;
#12780 = DIRECTION ( 'NONE',  ( 1.301042606982604138E-15, -1.000000000000000000, 0.000000000000000000 ) ) ;
#12781 = CARTESIAN_POINT ( 'NONE',  ( 1.214457691475989920, -3.869340823081270031, 2.684103622926340194 ) ) ;
#12782 = EDGE_CURVE ( 'NONE', #13986, #5262, #10667, .T. ) ;
#12783 = PLANE ( 'NONE',  #15863 ) ;
#12784 = CARTESIAN_POINT ( 'NONE',  ( 0.3429245540020083860, -3.776187669928120272, 2.675820019639898906 ) ) ;
#12785 = CARTESIAN_POINT ( 'NONE',  ( 7.069631497386979886E-16, 5.131370849898479136, 5.100000000000000533 ) ) ;
#12786 = CARTESIAN_POINT ( 'NONE',  ( 1.899999999999999911, 11.25000000000000000, 7.649999999999999467 ) ) ;
#12787 = VERTEX_POINT ( 'NONE', #13347 ) ;
#12788 = CARTESIAN_POINT ( 'NONE',  ( -0.5500000000000000444, 6.450000000000000178, 3.299999999999999822 ) ) ;
#12789 = VERTEX_POINT ( 'NONE', #3422 ) ;
#12790 = SURFACE_SIDE_STYLE ('',( #11304 ) ) ;
#12791 = ORIENTED_EDGE ( 'NONE', *, *, #12842, .T. ) ;
#12792 = CARTESIAN_POINT ( 'NONE',  ( 1.899999999999999911, 11.40000000000000036, 1.600000000000000089 ) ) ;
#12793 = VERTEX_POINT ( 'NONE', #14833 ) ;
#12794 = CARTESIAN_POINT ( 'NONE',  ( 1.782460458101500889, -5.099788135593215976, 5.718585207845976015 ) ) ;
#12795 = DIRECTION ( 'NONE',  ( 0.000000000000000000, -1.000000000000000000, 2.775557561562900226E-16 ) ) ;
#12796 = DIRECTION ( 'NONE',  ( -5.551115123125780730E-16, 0.000000000000000000, -1.000000000000000000 ) ) ;
#12797 = CARTESIAN_POINT ( 'NONE',  ( -0.3750000000000000000, 6.450000000000000178, 2.100000000000000089 ) ) ;
#12798 = CARTESIAN_POINT ( 'NONE',  ( -0.009452110982656879157, -5.299807955295460005, 2.350000000000000089 ) ) ;
#12799 = EDGE_CURVE ( 'NONE', #1178, #14262, #6494, .T. ) ;
#12800 = DIRECTION ( 'NONE',  ( 0.000000000000000000, -1.000000000000000000, 1.807003620809174385E-16 ) ) ;
#12801 = DIRECTION ( 'NONE',  ( -3.042833474898580443E-15, 3.289549702593060178E-16, 1.000000000000000000 ) ) ;
#12802 = CARTESIAN_POINT ( 'NONE',  ( -2.295719155670160383, -3.287133615874060055, 5.218091927917240191 ) ) ;
#12803 = CARTESIAN_POINT ( 'NONE',  ( 1.642659730162729925, -3.663587104846653730, 3.468508687188663675 ) ) ;
#12804 = CARTESIAN_POINT ( 'NONE',  ( 1.351903350398191206, -0.1156779661016950206, 6.245004350000406212 ) ) ;
#12805 = VECTOR ( 'NONE', #6003, 1000.000000000000000 ) ;
#12806 = LINE ( 'NONE', #10186, #12649 ) ;
#12807 = DIRECTION ( 'NONE',  ( 1.059965646700401283E-16, 0.6823182503600125903, 0.7310552682428677063 ) ) ;
#12808 = ORIENTED_EDGE ( 'NONE', *, *, #3469, .T. ) ;
#12809 = CARTESIAN_POINT ( 'NONE',  ( -1.713314936023349944, -0.2610169491525429764, 3.089913064446579760 ) ) ;
#12810 = CARTESIAN_POINT ( 'NONE',  ( -1.417709711196470046, -2.006277760018209566, 2.821478011237799954 ) ) ;
#12811 = ORIENTED_EDGE ( 'NONE', *, *, #17166, .F. ) ;
#12812 = ORIENTED_EDGE ( 'NONE', *, *, #4805, .T. ) ;
#12813 = EDGE_CURVE ( 'NONE', #14829, #10706, #7792, .T. ) ;
#12814 = CARTESIAN_POINT ( 'NONE',  ( -1.265407828724339767, -3.290974492234039595, 2.715689360385571405 ) ) ;
#12815 = APPLICATION_PROTOCOL_DEFINITION ( 'draft international standard', 'automotive_design', 1998, #7117 ) ;
#12816 = CARTESIAN_POINT ( 'NONE',  ( -2.653602652190420574, -5.524364406779660897, 4.735326402787099376 ) ) ;
#12817 = VERTEX_POINT ( 'NONE', #6587 ) ;
#12818 = CARTESIAN_POINT ( 'NONE',  ( 2.011500846714319835, -0.3489406779661020086, 3.478373409938460448 ) ) ;
#12819 = ORIENTED_EDGE ( 'NONE', *, *, #15769, .T. ) ;
#12820 = EDGE_CURVE ( 'NONE', #8080, #8437, #13441, .T. ) ;
#12821 = LINE ( 'NONE', #10307, #14663 ) ;
#12822 = CARTESIAN_POINT ( 'NONE',  ( -1.899999999999999911, 0.5999999999999999778, 7.599999999999999645 ) ) ;
#12823 = CARTESIAN_POINT ( 'NONE',  ( 1.764143222953819867, -2.425466949207401690, 3.649904513135025841 ) ) ;
#12824 = CARTESIAN_POINT ( 'NONE',  ( 1.554165089654128584, -0.4201271186440683758, 6.851145244874527584 ) ) ;
#12825 = EDGE_LOOP ( 'NONE', ( #13695, #2284, #125 ) ) ;
#12826 = DIRECTION ( 'NONE',  ( 1.746418240983389920E-16, -1.000000000000000000, 0.000000000000000000 ) ) ;
#12827 = CARTESIAN_POINT ( 'NONE',  ( 0.5372984490435490645, 4.250000000000000000, 7.700000000000000178 ) ) ;
#12828 = ORIENTED_EDGE ( 'NONE', *, *, #13770, .F. ) ;
#12829 = CARTESIAN_POINT ( 'NONE',  ( 0.002826310976700510246, -0.4052053642593020366, 2.204978094066170069 ) ) ;
#12830 = CARTESIAN_POINT ( 'NONE',  ( -1.351903350398179438, -5.484322033898315851, 6.245004350000422200 ) ) ;
#12831 = CARTESIAN_POINT ( 'NONE',  ( 2.318251751302029984, -0.06673728813559361150, 4.294764266798991592 ) ) ;
#12832 = CARTESIAN_POINT ( 'NONE',  ( -0.1565249325564300187, -5.453177966101690366, 7.048192310558509810 ) ) ;
#12833 = CARTESIAN_POINT ( 'NONE',  ( -1.221947981261169991, -0.5741044150835520332, 2.670403636935529956 ) ) ;
#12834 = ORIENTED_EDGE ( 'NONE', *, *, #9049, .F. ) ;
#12835 = CARTESIAN_POINT ( 'NONE',  ( -1.899999999999999911, 0.7500000000000000000, 7.649999999999999467 ) ) ;
#12836 = VECTOR ( 'NONE', #17551, 1000.000000000000000 ) ;
#12837 = CARTESIAN_POINT ( 'NONE',  ( 0.04278372834676710118, -1.870388906648450034, 2.346934926511239805 ) ) ;
#12838 = CARTESIAN_POINT ( 'NONE',  ( -0.1749999999999999889, 7.700000000000000178, 0.5999999999999999778 ) ) ;
#12839 = CARTESIAN_POINT ( 'NONE',  ( -0.4874850653659789645, -2.708767285026830951, 6.694306935672950765 ) ) ;
#12840 = CARTESIAN_POINT ( 'NONE',  ( -2.616666666666669805, -2.774341069716839796E-16, 7.649999999999999467 ) ) ;
#12841 = ORIENTED_EDGE ( 'NONE', *, *, #5686, .T. ) ;
#12842 = EDGE_CURVE ( 'NONE', #959, #13844, #3812, .T. ) ;
#12843 = CARTESIAN_POINT ( 'NONE',  ( 1.899999999999999911, 2.799999999999999822, 1.600000000000000089 ) ) ;
#12844 = CARTESIAN_POINT ( 'NONE',  ( -2.630358833876468960, -0.5313559322033900578, 4.347767980622416317 ) ) ;
#12845 = CARTESIAN_POINT ( 'NONE',  ( 0.5570002967656469961, -2.891232714973159812, 6.986590552960210587 ) ) ;
#12846 = CARTESIAN_POINT ( 'NONE',  ( 1.899999999999999911, 0.5999999999999999778, 7.550000000000000711 ) ) ;
#12847 = LINE ( 'NONE', #5807, #12731 ) ;
#12848 = CARTESIAN_POINT ( 'NONE',  ( 0.7998959936908462964, -5.135381355932194580, 7.230419212249866945 ) ) ;
#12849 = ORIENTED_EDGE ( 'NONE', *, *, #13471, .F. ) ;
#12850 = ORIENTED_EDGE ( 'NONE', *, *, #16927, .T. ) ;
#12851 = DIRECTION ( 'NONE',  ( 0.000000000000000000, 1.000000000000000000, 2.775557561562890365E-16 ) ) ;
#12852 =( NAMED_UNIT ( * ) SI_UNIT ( $, .STERADIAN. ) SOLID_ANGLE_UNIT ( ) );
#12853 = CARTESIAN_POINT ( 'NONE',  ( 0.000000000000000000, 0.000000000000000000, 0.000000000000000000 ) ) ;
#12854 = ORIENTED_EDGE ( 'NONE', *, *, #379, .T. ) ;
#12855 = EDGE_CURVE ( 'NONE', #5857, #5609, #17675, .T. ) ;
#12856 = CARTESIAN_POINT ( 'NONE',  ( 2.350000000000000089, -5.599999999999999645, 6.400000000000000355 ) ) ;
#12857 = CARTESIAN_POINT ( 'NONE',  ( -1.914021115237000137, -4.754295778036220277, 6.069404563272239983 ) ) ;
#12858 = DIRECTION ( 'NONE',  ( 1.000000000000000000, 0.000000000000000000, 0.000000000000000000 ) ) ;
#12859 = CARTESIAN_POINT ( 'NONE',  ( -1.899999999999999911, 0.5999999999999999778, 7.700000000000000178 ) ) ;
#12860 = AXIS2_PLACEMENT_3D ( 'NONE', #6468, #6650, #12304 ) ;
#12861 = CARTESIAN_POINT ( 'NONE',  ( -2.347833536521260367, -3.058091609351150097, 4.537447324629909851 ) ) ;
#12862 = DIRECTION ( 'NONE',  ( -2.220446049250309876E-16, 0.000000000000000000, 1.000000000000000000 ) ) ;
#12863 = CARTESIAN_POINT ( 'NONE',  ( -0.4790341583531910197, -3.683034516774959855, 2.395814251711740006 ) ) ;
#12864 = DIRECTION ( 'NONE',  ( 0.000000000000000000, 0.000000000000000000, 1.000000000000000000 ) ) ;
#12865 = CARTESIAN_POINT ( 'NONE',  ( -0.08304008649493913041, -2.961097579838030569, 6.751342532748503267 ) ) ;
#12866 = DIRECTION ( 'NONE',  ( -1.618168325422125073E-46, -1.000000000000000000, -1.110223024625159992E-16 ) ) ;
#12867 = EDGE_LOOP ( 'NONE', ( #6056, #11888, #3703, #8597, #4578, #9630, #7136, #2949 ) ) ;
#12868 = CARTESIAN_POINT ( 'NONE',  ( 0.5000000000000000000, 3.500000000000000000, 5.100000000000000533 ) ) ;
#12869 = ORIENTED_EDGE ( 'NONE', *, *, #16718, .F. ) ;
#12870 = EDGE_CURVE ( 'NONE', #17304, #13650, #6676, .T. ) ;
#12871 = CARTESIAN_POINT ( 'NONE',  ( 1.000000000000000000, -5.000000000000000000, 6.100000000000000533 ) ) ;
#12872 = ORIENTED_EDGE ( 'NONE', *, *, #8105, .F. ) ;
#12873 = LINE ( 'NONE', #9825, #2619 ) ;
#12874 = EDGE_CURVE ( 'NONE', #5170, #4541, #6951, .T. ) ;
#12875 = ORIENTED_EDGE ( 'NONE', *, *, #4708, .F. ) ;
#12876 = EDGE_CURVE ( 'NONE', #6139, #14118, #11030, .T. ) ;
#12877 = CARTESIAN_POINT ( 'NONE',  ( 1.695509042132770761, -5.346398305084745672, 3.542446458728613301 ) ) ;
#12878 = EDGE_CURVE ( 'NONE', #6927, #7652, #2519, .T. ) ;
#12879 = CARTESIAN_POINT ( 'NONE',  ( 2.435897774776379698, -2.359442960702510472, 5.753335522918191280 ) ) ;
#12880 = LINE ( 'NONE', #5478, #4057 ) ;
#12881 = DIRECTION ( 'NONE',  ( 0.000000000000000000, 0.000000000000000000, -1.000000000000000000 ) ) ;
#12882 = CARTESIAN_POINT ( 'NONE',  ( -0.5027094486773525661, -4.952022267818764867, 2.083735201298030137 ) ) ;
#12883 = DIRECTION ( 'NONE',  ( 1.224646799147350002E-16, -1.000000000000000000, -6.123233995736759873E-17 ) ) ;
#12884 = CARTESIAN_POINT ( 'NONE',  ( -1.399999999999999911, -5.500000000000000000, 5.100000000000000533 ) ) ;
#12885 = CARTESIAN_POINT ( 'NONE',  ( -1.507201387235980183, -3.124115597856050197, 6.507509243627219497 ) ) ;
#12886 = CARTESIAN_POINT ( 'NONE',  ( 1.079900583135640302, -3.570433951693503527, 2.953942563037689428 ) ) ;
#12887 = VECTOR ( 'NONE', #15312, 1000.000000000000000 ) ;
#12888 = CARTESIAN_POINT ( 'NONE',  ( -0.2812789908084309953, -0.1557203389830509876, 7.036533610117280624 ) ) ;
#12889 = LINE ( 'NONE', #3154, #10265 ) ;
#12890 = CARTESIAN_POINT ( 'NONE',  ( -1.695509042132779864, -0.5536016949152540167, 3.542446458728619518 ) ) ;
#12891 = DIRECTION ( 'NONE',  ( 0.3420201433256691015, 0.000000000000000000, 0.9396926207859082059 ) ) ;
#12892 = EDGE_LOOP ( 'NONE', ( #9865, #7250, #656, #5531 ) ) ;
#12893 = CARTESIAN_POINT ( 'NONE',  ( 2.180207327701309872, -0.09343220338983100615, 5.586116916730190063 ) ) ;
#12894 = CARTESIAN_POINT ( 'NONE',  ( 2.169623098572349917, -2.658349832090280529, 5.611855963200990338 ) ) ;
#12895 = EDGE_LOOP ( 'NONE', ( #5358, #6506, #13966, #8067 ) ) ;
#12896 = DIRECTION ( 'NONE',  ( 6.083413833562510128E-16, -1.647588903766459698E-16, 1.000000000000000000 ) ) ;
#12897 = EDGE_CURVE ( 'NONE', #6428, #17362, #8085, .T. ) ;
#12898 = ORIENTED_EDGE ( 'NONE', *, *, #15246, .T. ) ;
#12899 = CARTESIAN_POINT ( 'NONE',  ( 2.308170020371300257, -3.873181699441239800, 5.159452766389608591 ) ) ;
#12900 = CARTESIAN_POINT ( 'NONE',  ( 0.000000000000000000, 0.000000000000000000, 0.000000000000000000 ) ) ;
#12901 = CARTESIAN_POINT ( 'NONE',  ( 2.020286629067969297, -5.108686440677975504, 6.420841923842827370 ) ) ;
#12902 = VECTOR ( 'NONE', #280, 1000.000000000000000 ) ;
#12903 = EDGE_LOOP ( 'NONE', ( #10752, #7546, #4640, #1245 ) ) ;
#12904 = VECTOR ( 'NONE', #13239, 1000.000000000000000 ) ;
#12905 = CARTESIAN_POINT ( 'NONE',  ( 2.203023580853990193, -0.3578389830508479919, 3.872235369154280349 ) ) ;
#12906 = VERTEX_POINT ( 'NONE', #4080 ) ;
#12907 = DIRECTION ( 'NONE',  ( 7.273661547324610053E-16, -6.123233995736789455E-17, 1.000000000000000000 ) ) ;
#12908 = CARTESIAN_POINT ( 'NONE',  ( 0.7616804549307097938, -2.262448931189378509, 2.793499350326721142 ) ) ;
#12909 = VERTEX_POINT ( 'NONE', #2438 ) ;
#12910 = LINE ( 'NONE', #11696, #375 ) ;
#12911 = DIRECTION ( 'NONE',  ( 0.000000000000000000, 0.000000000000000000, -1.000000000000000000 ) ) ;
#12912 = CARTESIAN_POINT ( 'NONE',  ( 1.614765845140360589, -0.4067796610169500116, 5.967758800287426446 ) ) ;
#12913 = VECTOR ( 'NONE', #1532, 1000.000000000000000 ) ;
#12914 = ORIENTED_EDGE ( 'NONE', *, *, #7770, .F. ) ;
#12915 = DIRECTION ( 'NONE',  ( 0.7071067811865480168, 9.235837992257497283E-17, -0.7071067811865470176 ) ) ;
#12916 = CARTESIAN_POINT ( 'NONE',  ( 2.224278379903029901, -5.390889830508481140, 5.468825643806100700 ) ) ;
#12917 = LINE ( 'NONE', #245, #3797 ) ;
#12918 = EDGE_CURVE ( 'NONE', #8002, #2860, #16762, .T. ) ;
#12919 = CARTESIAN_POINT ( 'NONE',  ( -2.224278379903029457, -0.2091101694915259712, 5.468825643806110470 ) ) ;
#12920 = CARTESIAN_POINT ( 'NONE',  ( 1.899999999999999911, 7.299999999999999822, 1.600000000000000089 ) ) ;
#12921 = VECTOR ( 'NONE', #8661, 1000.000000000000000 ) ;
#12922 = VERTEX_POINT ( 'NONE', #5572 ) ;
#12923 = LINE ( 'NONE', #13016, #15606 ) ;
#12924 = CARTESIAN_POINT ( 'NONE',  ( -1.401708661791369881, -1.241605122864670063, 6.590491606684079962 ) ) ;
#12925 = AXIS2_PLACEMENT_3D ( 'NONE', #2779, #13972, #12780 ) ;
#12926 = DIRECTION ( 'NONE',  ( 6.123233995736769734E-17, 2.493473113004670213E-16, 1.000000000000000000 ) ) ;
#12927 = CIRCLE ( 'NONE', #503, 0.1499999999999999944 ) ;
#12928 = CARTESIAN_POINT ( 'NONE',  ( 0.4625564304288019568, -2.592325843585391532, 6.700235833919842676 ) ) ;
#12929 = DIRECTION ( 'NONE',  ( 1.000000000000000000, 1.189524669241239855E-16, 4.716563129111599823E-33 ) ) ;
#12930 = ORIENTED_EDGE ( 'NONE', *, *, #5458, .T. ) ;
#12931 = CIRCLE ( 'NONE', #3746, 1.000000000000000000 ) ;
#12932 = DIRECTION ( 'NONE',  ( 1.000000000000000000, 0.000000000000000000, 0.000000000000000000 ) ) ;
#12933 = CARTESIAN_POINT ( 'NONE',  ( -2.586172839791708533, -0.5358050847457624943, 4.104546363490954697 ) ) ;
#12934 = CARTESIAN_POINT ( 'NONE',  ( 1.401708661791409849, -4.358394877135329359, 6.590491606684049763 ) ) ;
#12935 = CYLINDRICAL_SURFACE ( 'NONE', #2774, 0.2500000000000002220 ) ;
#12936 = FACE_OUTER_BOUND ( 'NONE', #2750, .T. ) ;
#12937 = CARTESIAN_POINT ( 'NONE',  ( 0.07064654565475687875, -5.148728813559319661, 7.352897294663512717 ) ) ;
#12938 = VERTEX_POINT ( 'NONE', #16596 ) ;
#12939 = VECTOR ( 'NONE', #10979, 1000.000000000000000 ) ;
#12940 = AXIS2_PLACEMENT_3D ( 'NONE', #17339, #12926, #7380 ) ;
#12941 = ORIENTED_EDGE ( 'NONE', *, *, #16148, .T. ) ;
#12942 = PLANE ( 'NONE',  #1210 ) ;
#12943 = CARTESIAN_POINT ( 'NONE',  ( 1.632373740989790045, -0.7935201267648649415, 3.049747554812159755 ) ) ;
#12944 = ORIENTED_EDGE ( 'NONE', *, *, #4865, .F. ) ;
#12945 = VECTOR ( 'NONE', #6180, 1000.000000000000000 ) ;
#12946 = CARTESIAN_POINT ( 'NONE',  ( -2.091881088960070745, -1.610376859117309767, 6.333140288723886790 ) ) ;
#12947 = AXIS2_PLACEMENT_3D ( 'NONE', #7690, #4804, #17665 ) ;
#12948 = DIRECTION ( 'NONE',  ( 0.000000000000000000, 0.000000000000000000, 1.000000000000000000 ) ) ;
#12949 = CARTESIAN_POINT ( 'NONE',  ( -0.5500000000000000444, 2.050000000000000266, 1.600000000000000089 ) ) ;
#12950 = CARTESIAN_POINT ( 'NONE',  ( 2.062913653388430024, -2.382731248990799688, 5.832754583370790336 ) ) ;
#12951 = CARTESIAN_POINT ( 'NONE',  ( 1.661700935788380074, -5.037500000000000533, 3.038299064211610112 ) ) ;
#12952 = AXIS2_PLACEMENT_3D ( 'NONE', #990, #13681, #6627 ) ;
#12953 = CARTESIAN_POINT ( 'NONE',  ( -1.752195476665039831, -1.563800282540731779, 6.693219682964347328 ) ) ;
#12954 = DIRECTION ( 'NONE',  ( 0.000000000000000000, -1.000000000000000000, 0.000000000000000000 ) ) ;
#12955 = CARTESIAN_POINT ( 'NONE',  ( -1.861802609626409089, -4.800872354612795156, 5.565212624397245733 ) ) ;
#12956 = CARTESIAN_POINT ( 'NONE',  ( -2.143090896833110381, -0.5046610169491529962, 5.672454929438350391 ) ) ;
#12957 = DIRECTION ( 'NONE',  ( 0.9622640697945186172, -0.2721173643531222264, 0.000000000000000000 ) ) ;
#12958 = VECTOR ( 'NONE', #8435, 1000.000000000000000 ) ;
#12959 = DIRECTION ( 'NONE',  ( 1.480297366166879989E-15, 1.000000000000000000, 0.000000000000000000 ) ) ;
#12960 = EDGE_LOOP ( 'NONE', ( #4248, #17356, #13301, #16881 ) ) ;
#12961 = VECTOR ( 'NONE', #938, 1000.000000000000000 ) ;
#12962 = DIRECTION ( 'NONE',  ( 0.000000000000000000, -1.000000000000000000, -8.540177112501209562E-17 ) ) ;
#12963 = ORIENTED_EDGE ( 'NONE', *, *, #148, .T. ) ;
#12964 = PLANE ( 'NONE',  #11154 ) ;
#12965 = CARTESIAN_POINT ( 'NONE',  ( 1.800000000000000044, 11.40000000000000036, 7.550000000000000711 ) ) ;
#12966 = VECTOR ( 'NONE', #2238, 1000.000000000000114 ) ;
#12967 = ORIENTED_EDGE ( 'NONE', *, *, #14756, .F. ) ;
#12968 = CARTESIAN_POINT ( 'NONE',  ( 1.134881315981519645, -5.422033898305085309, 6.410767520434657918 ) ) ;
#12969 = CARTESIAN_POINT ( 'NONE',  ( -1.901407128523849632, -2.848497014756559143, 6.551422324754827109 ) ) ;
#12970 = FACE_OUTER_BOUND ( 'NONE', #15754, .T. ) ;
#12971 = FACE_OUTER_BOUND ( 'NONE', #50, .T. ) ;
#12972 = VECTOR ( 'NONE', #8591, 1000.000000000000000 ) ;
#12973 = LINE ( 'NONE', #296, #12904 ) ;
#12974 = VECTOR ( 'NONE', #298, 1000.000000000000000 ) ;
#12975 = CARTESIAN_POINT ( 'NONE',  ( -1.899999999999999911, 9.199999999999999289, 0.6099999999999999867 ) ) ;
#12976 = CARTESIAN_POINT ( 'NONE',  ( 1.800000000000000044, 7.799999999999999822, 7.599999999999999645 ) ) ;
#12977 = CARTESIAN_POINT ( 'NONE',  ( -2.351999299633229956, -3.333710192450639820, 4.782734406438290620 ) ) ;
#12978 = CARTESIAN_POINT ( 'NONE',  ( 1.790316459643169100, -0.8651516338920848259, 3.695177221627173214 ) ) ;
#12979 = EDGE_CURVE ( 'NONE', #13315, #1371, #2704, .T. ) ;
#12980 = CARTESIAN_POINT ( 'NONE',  ( -1.811729841638700211, -0.2580508474576269640, 3.197954009834299782 ) ) ;
#12981 = CARTESIAN_POINT ( 'NONE',  ( 2.500000000000000000, 10.00000000000000000, 1.600000000000000089 ) ) ;
#12982 = ADVANCED_FACE ( 'NONE', ( #8354 ), #15212, .T. ) ;
#12983 = CARTESIAN_POINT ( 'NONE',  ( 3.673940397442059498E-17, 3.581751045813930112, 8.000000000000000000 ) ) ;
#12984 = ORIENTED_EDGE ( 'NONE', *, *, #11113, .T. ) ;
#12985 = CARTESIAN_POINT ( 'NONE',  ( 0.9490039995898825742, -3.523857375116919322, 2.221592224478729172 ) ) ;
#12986 = CARTESIAN_POINT ( 'NONE',  ( -1.782460458101500889, -0.2002118644067801267, 5.718585207845990226 ) ) ;
#12987 = CARTESIAN_POINT ( 'NONE',  ( 1.353103843060669886, -2.798079561820010053, 6.625579309552930063 ) ) ;
#12988 = VERTEX_POINT ( 'NONE', #9635 ) ;
#12989 = VECTOR ( 'NONE', #5039, 1000.000000000000000 ) ;
#12990 = ORIENTED_EDGE ( 'NONE', *, *, #1598, .F. ) ;
#12991 = CARTESIAN_POINT ( 'NONE',  ( -1.902324933209428970, -3.197821339080880509, 3.314393441133570484 ) ) ;
#12992 = DIRECTION ( 'NONE',  ( 1.000000000000000000, 0.000000000000000000, 0.000000000000000000 ) ) ;
#12993 = CARTESIAN_POINT ( 'NONE',  ( -2.560337424259679917, -5.237711864406785267, 4.001768473655595848 ) ) ;
#12994 = ORIENTED_EDGE ( 'NONE', *, *, #15426, .T. ) ;
#12995 = LINE ( 'NONE', #11879, #12044 ) ;
#12996 = CARTESIAN_POINT ( 'NONE',  ( -0.06264882350515391107, -0.4512711864406790396, 7.052569299041220319 ) ) ;
#12997 = ORIENTED_EDGE ( 'NONE', *, *, #7560, .T. ) ;
#12998 = EDGE_CURVE ( 'NONE', #2042, #11364, #1132, .T. ) ;
#12999 = CARTESIAN_POINT ( 'NONE',  ( -1.300000000000000044, 1.592040838891560081E-16, 7.599999999999999645 ) ) ;
#13000 = AXIS2_PLACEMENT_3D ( 'NONE', #12144, #6768, #17763 ) ;
#13001 = CARTESIAN_POINT ( 'NONE',  ( -1.798783563193318891, -3.217268751009201289, 5.689585537188996511 ) ) ;
#13003 = EDGE_CURVE ( 'NONE', #13806, #6568, #3899, .T. ) ;
#13002 = LINE ( 'NONE', #14381, #1116 ) ;
#13004 = ORIENTED_EDGE ( 'NONE', *, *, #17183, .T. ) ;
#13005 = FACE_OUTER_BOUND ( 'NONE', #5708, .T. ) ;
#13006 = ADVANCED_FACE ( 'NONE', ( #5475 ), #2614, .F. ) ;
#13007 = DIRECTION ( 'NONE',  ( -1.000000000000000000, 0.000000000000000000, 0.000000000000000000 ) ) ;
#13008 = LINE ( 'NONE', #17852, #1092 ) ;
#13009 = ORIENTED_EDGE ( 'NONE', *, *, #15378, .T. ) ;
#13010 = CARTESIAN_POINT ( 'NONE',  ( -0.002227590684724169937, -0.4853054260922249896, 2.202374039106750114 ) ) ;
#13011 = CARTESIAN_POINT ( 'NONE',  ( 2.350067830300900162, -5.377542372881360500, 4.825253242917690422 ) ) ;
#13012 = CARTESIAN_POINT ( 'NONE',  ( 0.5889081234606849957, -0.1379237288135600759, 6.978529000034869867 ) ) ;
#13013 = CIRCLE ( 'NONE', #5019, 1.000000000000000000 ) ;
#13014 = CARTESIAN_POINT ( 'NONE',  ( -1.449852972480019764, -3.589881363621813648, 2.477154964647171109 ) ) ;
#13015 = ORIENTED_EDGE ( 'NONE', *, *, #3281, .F. ) ;
#13016 = CARTESIAN_POINT ( 'NONE',  ( -1.899999999999999911, 2.000000000000000000, -2.537652627714639929E-16 ) ) ;
#13017 = CARTESIAN_POINT ( 'NONE',  ( 2.283153923255319739, -2.196424942684489512, 4.129076318403449797 ) ) ;
#13018 = LINE ( 'NONE', #17437, #8214 ) ;
#13019 = CARTESIAN_POINT ( 'NONE',  ( 1.279347147864559275, -2.033406924666469884, 3.094331068408280760 ) ) ;
#13021 = EDGE_CURVE ( 'NONE', #37, #4379, #8264, .T. ) ;
#13020 = LINE ( 'NONE', #6061, #4634 ) ;
#13022 = VERTEX_POINT ( 'NONE', #12596 ) ;
#13023 = VECTOR ( 'NONE', #8743, 1000.000000000000000 ) ;
#13024 = LINE ( 'NONE', #15898, #6155 ) ;
#13025 = CARTESIAN_POINT ( 'NONE',  ( -2.239137794397029868, -4.987178660919110662, 3.975425900939220103 ) ) ;
#13026 = CARTESIAN_POINT ( 'NONE',  ( -2.500000000000000000, 2.000000000000000000, 1.600000000000000089 ) ) ;
#13027 = LINE ( 'NONE', #7290, #3270 ) ;
#13028 = CARTESIAN_POINT ( 'NONE',  ( -0.7322514394120432923, -5.286652542372874741, 2.149183891723918993 ) ) ;
#13029 = ORIENTED_EDGE ( 'NONE', *, *, #17323, .F. ) ;
#13030 = ORIENTED_EDGE ( 'NONE', *, *, #5201, .F. ) ;
#13031 = CARTESIAN_POINT ( 'NONE',  ( -4.592425496802619825E-17, 2.550000000000000266, 5.100000000000000533 ) ) ;
#13032 = CARTESIAN_POINT ( 'NONE',  ( -1.889999999999999902, 4.100000000000000533, 0.5999999999999999778 ) ) ;
#13033 = ORIENTED_EDGE ( 'NONE', *, *, #9248, .F. ) ;
#13034 = EDGE_CURVE ( 'NONE', #12167, #5801, #15402, .T. ) ;
#13035 = VECTOR ( 'NONE', #13964, 1000.000000000000000 ) ;
#13036 = PLANE ( 'NONE',  #11203 ) ;
#13037 = CARTESIAN_POINT ( 'NONE',  ( -2.135041058613629694, -4.800872354612799597, 5.690123914223820023 ) ) ;
#13038 = CARTESIAN_POINT ( 'NONE',  ( 0.009452110982655428928, -0.3001920447045380858, 2.649999999999998579 ) ) ;
#13039 = CARTESIAN_POINT ( 'NONE',  ( -1.149999999999999911, 9.299999999999998934, 7.700000000000000178 ) ) ;
#13040 = CARTESIAN_POINT ( 'NONE',  ( -1.167621112247339887, -2.778632149891699932, 6.743381174846780013 ) ) ;
#13042 = EDGE_CURVE ( 'NONE', #8865, #5991, #1220, .T. ) ;
#13041 = CARTESIAN_POINT ( 'NONE',  ( 0.5677251586959709551, -5.311531839079339790, 2.399563163165729929 ) ) ;
#13043 = CARTESIAN_POINT ( 'NONE',  ( 2.510208264419000468, -1.074746228486680000, 5.561375738133185642 ) ) ;
#13044 = DIRECTION ( 'NONE',  ( 0.000000000000000000, -1.000000000000000000, -1.387778780781439759E-16 ) ) ;
#13045 = LINE ( 'NONE', #11745, #4646 ) ;
#13046 = CARTESIAN_POINT ( 'NONE',  ( 1.065036425888030713, -4.381683165423609694, 6.455163597548602361 ) ) ;
#13047 = CARTESIAN_POINT ( 'NONE',  ( -1.925796468768790071, -0.4957627118644070130, 6.052706598917719560 ) ) ;
#13048 = DIRECTION ( 'NONE',  ( -3.700743415417190309E-15, 0.000000000000000000, -1.000000000000000000 ) ) ;
#13049 = LINE ( 'NONE', #13313, #18012 ) ;
#13050 = EDGE_LOOP ( 'NONE', ( #1472, #1833, #9736, #6341 ) ) ;
#13051 = FACE_OUTER_BOUND ( 'NONE', #14099, .T. ) ;
#13052 = ORIENTED_EDGE ( 'NONE', *, *, #16050, .F. ) ;
#13053 = CARTESIAN_POINT ( 'NONE',  ( 1.000000000000000000, 5.400000000000000355, 7.700000000000000178 ) ) ;
#13054 = CARTESIAN_POINT ( 'NONE',  ( -0.1749999999999999889, 7.500000000000000000, 1.600000000000000089 ) ) ;
#13055 = ORIENTED_EDGE ( 'NONE', *, *, #13786, .F. ) ;
#13056 = CARTESIAN_POINT ( 'NONE',  ( 1.580445181003960586, -5.341949152542365908, 3.389704561770334301 ) ) ;
#13057 = CARTESIAN_POINT ( 'NONE',  ( 8.782273797403119722E-16, 6.262741699796950279, 6.100000000000000533 ) ) ;
#13058 = DIRECTION ( 'NONE',  ( 0.000000000000000000, 0.000000000000000000, -1.000000000000000000 ) ) ;
#13059 = CARTESIAN_POINT ( 'NONE',  ( 0.8400312909773258729, -2.569037555297099651, 7.217431453521787610 ) ) ;
#13060 = SURFACE_STYLE_USAGE ( .BOTH. , #8887 ) ;
#13061 = CARTESIAN_POINT ( 'NONE',  ( 1.740526006427820072, -0.5337085751346559714, 2.973047620154039894 ) ) ;
#13062 = DIRECTION ( 'NONE',  ( 6.123233995736767268E-17, 1.000000000000000000, 0.000000000000000000 ) ) ;
#13063 = CARTESIAN_POINT ( 'NONE',  ( 2.145694642186089851, -1.098034516774969882, 5.666819626392539888 ) ) ;
#13064 = LINE ( 'NONE', #716, #6463 ) ;
#13065 = CARTESIAN_POINT ( 'NONE',  ( -1.777964140657649850, -4.731007489747940831, 6.241943319976260618 ) ) ;
#13066 = CARTESIAN_POINT ( 'NONE',  ( -0.6217226704572171858, -4.292370888630430592, 6.656620240022991908 ) ) ;
#13067 = CARTESIAN_POINT ( 'NONE',  ( 0.3265524029357661506, -0.1423728813559330397, 6.726831181542982208 ) ) ;
#13068 = DIRECTION ( 'NONE',  ( 1.000000000000000000, 0.000000000000000000, 0.000000000000000000 ) ) ;
#13069 = EDGE_CURVE ( 'NONE', #8102, #4320, #11115, .T. ) ;
#13070 = CARTESIAN_POINT ( 'NONE',  ( -1.800000000000000044, 11.40000000000000036, 6.599999999999999645 ) ) ;
#13071 = EDGE_LOOP ( 'NONE', ( #80, #1391, #8749, #2530 ) ) ;
#13072 = CARTESIAN_POINT ( 'NONE',  ( 2.121170185508189476, -3.663587104846653730, 3.105085978143951486 ) ) ;
#13073 = CARTESIAN_POINT ( 'NONE',  ( 1.754713504580569960, -0.04894067796610205440, 3.634325740584615883 ) ) ;
#13074 = CARTESIAN_POINT ( 'NONE',  ( 2.347833536521260367, -2.541908390648839777, 4.537447324629859224 ) ) ;
#13075 = ORIENTED_EDGE ( 'NONE', *, *, #86, .F. ) ;
#13076 = ORIENTED_EDGE ( 'NONE', *, *, #14580, .F. ) ;
#13077 = ORIENTED_EDGE ( 'NONE', *, *, #6108, .T. ) ;
#13078 = CARTESIAN_POINT ( 'NONE',  ( -1.611907055891630414, -3.244397915657460274, 2.985210995296890601 ) ) ;
#13079 = APPLICATION_PROTOCOL_DEFINITION ( 'draft international standard', 'automotive_design', 1998, #7798 ) ;
#13080 = CARTESIAN_POINT ( 'NONE',  ( 1.467041701146838406, -5.122033898305085486, 6.911479965439912831 ) ) ;
#13081 = DIRECTION ( 'NONE',  ( 1.000000000000000000, 0.000000000000000000, 0.000000000000000000 ) ) ;
#13082 = VECTOR ( 'NONE', #8421, 1000.000000000000000 ) ;
#13083 = ORIENTED_EDGE ( 'NONE', *, *, #12318, .T. ) ;
#13084 = LINE ( 'NONE', #13260, #2588 ) ;
#13085 = ADVANCED_FACE ( 'NONE', ( #6643 ), #13501, .T. ) ;
#13086 = CARTESIAN_POINT ( 'NONE',  ( -1.641808337277740115, -0.4868644067796619734, 6.386111670537629514 ) ) ;
#13087 = EDGE_LOOP ( 'NONE', ( #14875, #15834, #6433, #14554 ) ) ;
#13088 = FACE_OUTER_BOUND ( 'NONE', #3255, .T. ) ;
#13089 = CARTESIAN_POINT ( 'NONE',  ( 1.250000000000000000, 3.500000000000000000, 5.100000000000000533 ) ) ;
#13090 = CARTESIAN_POINT ( 'NONE',  ( -2.049636678546640667, -3.356998480738929924, 4.582138519505405405 ) ) ;
#13091 = CARTESIAN_POINT ( 'NONE',  ( 0.08231150243515643339, -0.001483050847457899508, 2.050000000000001155 ) ) ;
#13092 = ORIENTED_EDGE ( 'NONE', *, *, #16940, .F. ) ;
#13093 = CARTESIAN_POINT ( 'NONE',  ( -1.850000000000000089, 0.7500000000000000000, 7.649999999999999467 ) ) ;
#13094 = CARTESIAN_POINT ( 'NONE',  ( 0.3265524029357661506, -0.4423728813559331119, 6.726831181542982208 ) ) ;
#13095 = ADVANCED_FACE ( 'NONE', ( #9138 ), #17919, .T. ) ;
#13096 = VERTEX_POINT ( 'NONE', #720 ) ;
#13097 = CARTESIAN_POINT ( 'NONE',  ( 2.500000000000000000, 2.000000000000000000, -1.695950706916410117E-15 ) ) ;
#13098 = CARTESIAN_POINT ( 'NONE',  ( 2.143090896833110381, -5.395338983050850246, 5.672454929438339732 ) ) ;
#13099 =( LENGTH_UNIT ( ) NAMED_UNIT ( * ) SI_UNIT ( .MILLI., .METRE. ) );
#13100 = EDGE_CURVE ( 'NONE', #9757, #13610, #7760, .T. ) ;
#13101 = VECTOR ( 'NONE', #4228, 1000.000000000000000 ) ;
#13102 = PLANE ( 'NONE',  #3555 ) ;
#13103 = PRODUCT_RELATED_PRODUCT_CATEGORY ( 'part', '', ( #7704 ) ) ;
#13104 = ADVANCED_FACE ( 'NONE', ( #1006 ), #14797, .F. ) ;
#13105 = CARTESIAN_POINT ( 'NONE',  ( -0.04661003995944364847, -3.729611093351542284, 2.046522810126899294 ) ) ;
#13106 = ORIENTED_EDGE ( 'NONE', *, *, #9489, .T. ) ;
#13107 = EDGE_CURVE ( 'NONE', #16569, #15379, #8136, .T. ) ;
#13108 = CARTESIAN_POINT ( 'NONE',  ( -1.353103843060629918, -2.801920438179979822, 6.625579309552960261 ) ) ;
#13109 = EDGE_CURVE ( 'NONE', #12574, #9877, #10521, .T. ) ;
#13110 = CARTESIAN_POINT ( 'NONE',  ( -1.899999999999999911, 11.29999999999999893, 1.600000000000000089 ) ) ;
#13111 = CYLINDRICAL_SURFACE ( 'NONE', #5412, 0.04999999999999969746 ) ;
#13112 = EDGE_CURVE ( 'NONE', #15044, #2252, #9433, .T. ) ;
#13113 = CARTESIAN_POINT ( 'NONE',  ( -1.019987577504920528, -2.778632149891700376, 6.481720287913836920 ) ) ;
#13114 = DIRECTION ( 'NONE',  ( -1.000000000000000000, 0.000000000000000000, 0.000000000000000000 ) ) ;
#13115 = CIRCLE ( 'NONE', #6903, 0.1000000000000000472 ) ;
#13116 = VERTEX_POINT ( 'NONE', #15097 ) ;
#13117 = CARTESIAN_POINT ( 'NONE',  ( -0.03000000000000000236, 11.40000000000000036, 6.759657321199410264E-76 ) ) ;
#13118 = CARTESIAN_POINT ( 'NONE',  ( -2.608006145151089861, -1.427911429170979352, 5.191342690854409803 ) ) ;
#13119 = CARTESIAN_POINT ( 'NONE',  ( -0.8244235255442939891, -0.5829339996946389935, 2.492493020344019872 ) ) ;
#13120 = CARTESIAN_POINT ( 'NONE',  ( -0.1749999999999999889, 7.700000000000000178, 1.600000000000000089 ) ) ;
#13121 = DIRECTION ( 'NONE',  ( 1.224646799147350002E-16, -1.000000000000000000, -6.123233995736769734E-17 ) ) ;
#13122 = CARTESIAN_POINT ( 'NONE',  ( 2.350067830300900162, -5.077542372881360677, 4.825253242917690422 ) ) ;
#13123 = ORIENTED_EDGE ( 'NONE', *, *, #4253, .F. ) ;
#13124 = ORIENTED_EDGE ( 'NONE', *, *, #18114, .T. ) ;
#13125 = DIRECTION ( 'NONE',  ( -1.000000000000000000, 0.000000000000000000, 0.000000000000000000 ) ) ;
#13126 = VECTOR ( 'NONE', #17743, 1000.000000000000000 ) ;
#13127 = LINE ( 'NONE', #14597, #17936 ) ;
#13128 = EDGE_CURVE ( 'NONE', #15430, #2341, #17547, .T. ) ;
#13129 = EDGE_LOOP ( 'NONE', ( #471, #3962, #5779, #11353 ) ) ;
#13130 = CARTESIAN_POINT ( 'NONE',  ( 2.594645788401200637, -2.611773255513701653, 5.257608218854235460 ) ) ;
#13131 = CARTESIAN_POINT ( 'NONE',  ( 0.2151249875495270247, -0.3251990024832489556, 2.650810719223910983 ) ) ;
#13132 = CARTESIAN_POINT ( 'NONE',  ( -1.000000000000000000, -8.000000000000000000, 5.700000000000000178 ) ) ;
#13133 = CARTESIAN_POINT ( 'NONE',  ( -1.866416942370660026, -1.637506023765569863, 3.266391446483499994 ) ) ;
#13134 = LINE ( 'NONE', #14336, #13809 ) ;
#13135 = CARTESIAN_POINT ( 'NONE',  ( 2.418933091173299577, -1.098034516774970770, 5.791730916219126613 ) ) ;
#13136 = DIRECTION ( 'NONE',  ( 0.000000000000000000, 0.000000000000000000, 1.000000000000000000 ) ) ;
#13137 = CARTESIAN_POINT ( 'NONE',  ( 0.8967027089123184025, -4.404971453711897134, 6.546842195331636916 ) ) ;
#13138 = CARTESIAN_POINT ( 'NONE',  ( 2.353194804772640314, -0.3756355932203400139, 4.731327187377229571 ) ) ;
#13139 = DIRECTION ( 'NONE',  ( -6.740754805355319355E-31, 1.000000000000000000, -1.040834085586083310E-14 ) ) ;
#13140 = EDGE_LOOP ( 'NONE', ( #4186, #5136, #10721 ) ) ;
#13141 = CARTESIAN_POINT ( 'NONE',  ( -0.1749999999999999889, 5.200000000000000178, 0.5999999999999999778 ) ) ;
#13142 = ORIENTED_EDGE ( 'NONE', *, *, #4805, .F. ) ;
#13143 = CARTESIAN_POINT ( 'NONE',  ( -1.399999999999999911, 5.799999999999999822, 8.300000000000000711 ) ) ;
#13144 = DIRECTION ( 'NONE',  ( 0.000000000000000000, 0.000000000000000000, -1.000000000000000000 ) ) ;
#13145 = EDGE_CURVE ( 'NONE', #3506, #9728, #17742, .T. ) ;
#13146 = VERTEX_POINT ( 'NONE', #6556 ) ;
#13147 = CARTESIAN_POINT ( 'NONE',  ( 2.322440385110930094, -2.518620102360550117, 4.319189883157390497 ) ) ;
#13148 = CARTESIAN_POINT ( 'NONE',  ( 1.899999999999999911, 0.7211102550927980248, 4.000000000000000000 ) ) ;
#13149 = CARTESIAN_POINT ( 'NONE',  ( -0.5500000000000000444, 3.050000000000000266, 3.399999999999999911 ) ) ;
#13150 = CARTESIAN_POINT ( 'NONE',  ( -0.1749999999999999889, 9.299999999999998934, 0.4000000000000000222 ) ) ;
#13151 = CARTESIAN_POINT ( 'NONE',  ( -0.8001898266890440370, -1.470647129387580021, 6.913242401714570384 ) ) ;
#13152 = CARTESIAN_POINT ( 'NONE',  ( -1.688800633088611836, -4.758136654396205145, 3.532586505616431616 ) ) ;
#13153 = CARTESIAN_POINT ( 'NONE',  ( -2.500000000000000000, 4.700000000000000178, 1.600000000000000089 ) ) ;
#13154 = FACE_OUTER_BOUND ( 'NONE', #17837, .T. ) ;
#13155 = ORIENTED_EDGE ( 'NONE', *, *, #6580, .F. ) ;
#13156 = CARTESIAN_POINT ( 'NONE',  ( 0.5137283630188955730, -0.1379237288135599648, 6.687652957477222770 ) ) ;
#13157 = CARTESIAN_POINT ( 'NONE',  ( 0.8242394280877100021, -4.428259742000189902, 6.904399023015010073 ) ) ;
#13158 = EDGE_LOOP ( 'NONE', ( #12129, #11522, #9029 ) ) ;
#13159 = ORIENTED_EDGE ( 'NONE', *, *, #7896, .T. ) ;
#13160 = CARTESIAN_POINT ( 'NONE',  ( 0.4000000000000000222, -1.399999999999999911, 6.100000000000000533 ) ) ;
#13161 = EDGE_LOOP ( 'NONE', ( #8211, #7674, #14382, #16793 ) ) ;
#13162 = CARTESIAN_POINT ( 'NONE',  ( -2.126557263589649249, -3.151244762504310071, 3.691783806836060222 ) ) ;
#13163 = APPLICATION_PROTOCOL_DEFINITION ( 'draft international standard', 'automotive_design', 1998, #244 ) ;
#13164 = CARTESIAN_POINT ( 'NONE',  ( 1.666450993087180477, -5.117584745762705722, 6.765380371283858274 ) ) ;
#13165 = DIRECTION ( 'NONE',  ( -0.7071067811865480168, -0.7071067811865470176, 0.000000000000000000 ) ) ;
#13166 = VECTOR ( 'NONE', #13719, 1000.000000000000000 ) ;
#13167 = CARTESIAN_POINT ( 'NONE',  ( -2.332582362116870200, -0.5313559322033900578, 4.387643303570819775 ) ) ;
#13168 = EDGE_CURVE ( 'NONE', #13931, #7939, #5072, .T. ) ;
#13169 = VERTEX_POINT ( 'NONE', #16280 ) ;
#13170 = FACE_OUTER_BOUND ( 'NONE', #18186, .T. ) ;
#13171 = CARTESIAN_POINT ( 'NONE',  ( -1.549925137359298599, -4.731007489747939054, 6.046340934239856857 ) ) ;
#13172 = CARTESIAN_POINT ( 'NONE',  ( 0.4221287159901364605, -0.4423728813559331119, 7.320050063945812369 ) ) ;
#13173 = EDGE_LOOP ( 'NONE', ( #16698, #1199, #16628, #10992 ) ) ;
#13174 = CARTESIAN_POINT ( 'NONE',  ( 1.800000000000000044, 0.5999999999999999778, 1.600000000000000089 ) ) ;
#13175 = VERTEX_POINT ( 'NONE', #16563 ) ;
#13176 = CARTESIAN_POINT ( 'NONE',  ( -0.004607033757061119485, -0.5230175839438470087, 2.216967106706559498 ) ) ;
#13177 = CARTESIAN_POINT ( 'NONE',  ( -0.8570167067220350043, -5.582203389830509899, 2.508190348879359988 ) ) ;
#13179 = AXIS2_PLACEMENT_3D ( 'NONE', #15114, #7977, #9543 ) ;
#13178 = CARTESIAN_POINT ( 'NONE',  ( 1.399999999999999911, -5.000000000000000000, 6.100000000000000533 ) ) ;
#13180 = CARTESIAN_POINT ( 'NONE',  ( -2.043308330018789309, -0.2002118644067800435, 5.867646457774671198 ) ) ;
#13181 = VECTOR ( 'NONE', #2425, 1000.000000000000000 ) ;
#13182 = CARTESIAN_POINT ( 'NONE',  ( -2.161103922260861232, -3.496728210468663889, 3.159628768708461877 ) ) ;
#13183 = VERTEX_POINT ( 'NONE', #16370 ) ;
#13184 = CARTESIAN_POINT ( 'NONE',  ( -2.023259452208839626, -3.174533050792599731, 3.497849062500260064 ) ) ;
#13185 = CARTESIAN_POINT ( 'NONE',  ( -0.2335786437626909962, 6.450000000000000178, 2.241421356237310203 ) ) ;
#13186 = DIRECTION ( 'NONE',  ( -1.000000000000000000, 0.000000000000000000, 0.000000000000000000 ) ) ;
#13187 = CARTESIAN_POINT ( 'NONE',  ( -0.01333550863832440661, -3.430704221963769562, 2.647020699851690306 ) ) ;
#13188 = CARTESIAN_POINT ( 'NONE',  ( -2.500000000000000000, 9.199999999999999289, 1.600000000000000089 ) ) ;
#13189 = DIRECTION ( 'NONE',  ( -1.000000000000000000, 0.000000000000000000, 0.000000000000000000 ) ) ;
#13190 = AXIS2_PLACEMENT_3D ( 'NONE', #11690, #8651, #8914 ) ;
#13191 = CARTESIAN_POINT ( 'NONE',  ( 1.117157304995380240, -0.9388573751169233539, 6.422457952614097465 ) ) ;
#13192 = EDGE_LOOP ( 'NONE', ( #4827, #14016, #865, #18188 ) ) ;
#13193 = EDGE_CURVE ( 'NONE', #13368, #11846, #10812, .T. ) ;
#13194 = CARTESIAN_POINT ( 'NONE',  ( -0.2335786437626909962, 3.050000000000000266, 2.241421356237310203 ) ) ;
#13195 = ADVANCED_FACE ( 'NONE', ( #3675 ), #12298, .T. ) ;
#13196 = ORIENTED_EDGE ( 'NONE', *, *, #4194, .F. ) ;
#13197 = CARTESIAN_POINT ( 'NONE',  ( -0.1869574461324000070, -0.5962015548080630278, 2.350675676344399889 ) ) ;
#13198 = CARTESIAN_POINT ( 'NONE',  ( -0.5999999999999999778, 11.40000000000000036, 7.599999999999999645 ) ) ;
#13199 = EDGE_CURVE ( 'NONE', #1946, #16101, #6354, .T. ) ;
#13200 = DIRECTION ( 'NONE',  ( -0.7071067811865502373, 0.000000000000000000, -0.7071067811865447972 ) ) ;
#13201 = CARTESIAN_POINT ( 'NONE',  ( 0.7093417302541469294, -5.135381355932199909, 6.943956659919690466 ) ) ;
#13202 = VERTEX_POINT ( 'NONE', #7850 ) ;
#13203 = ORIENTED_EDGE ( 'NONE', *, *, #7009, .T. ) ;
#13204 = LINE ( 'NONE', #525, #1813 ) ;
#13205 = SHAPE_REPRESENTATION_RELATIONSHIP ( 'NONE' , 'NONE' ,  #2146, #15507 ) ;
#13206 = VECTOR ( 'NONE', #1310, 1000.000000000000000 ) ;
#13207 = ORIENTED_EDGE ( 'NONE', *, *, #14173, .F. ) ;
#13208 = CIRCLE ( 'NONE', #12635, 0.2500000000000006106 ) ;
#13209 = AXIS2_PLACEMENT_3D ( 'NONE', #3690, #17659, #4997 ) ;
#13210 = VECTOR ( 'NONE', #10261, 1000.000000000000000 ) ;
#13211 = CARTESIAN_POINT ( 'NONE',  ( 1.524497189778211581, -2.798079561820010941, 6.872331008700157007 ) ) ;
#13212 = CARTESIAN_POINT ( 'NONE',  ( 1.159526867004269768, -0.4480353997208165184, 2.996084454861921209 ) ) ;
#13213 = DIRECTION ( 'NONE',  ( -2.220446049250309876E-16, -1.000000000000000000, -2.902774059941839988E-17 ) ) ;
#13214 = CARTESIAN_POINT ( 'NONE',  ( -0.8189529353761560992, -1.777235753495300052, 2.493631540942749858 ) ) ;
#13215 = CARTESIAN_POINT ( 'NONE',  ( 0.8611469534735395337, -5.020626044399135068, 2.833474624362548600 ) ) ;
#13216 = ADVANCED_FACE ( 'NONE', ( #9322 ), #2307, .T. ) ;
#13217 = CARTESIAN_POINT ( 'NONE',  ( -2.218077401483159683, -4.824160642901089702, 5.486688202856539576 ) ) ;
#13218 = LINE ( 'NONE', #13666, #17312 ) ;
#13219 = CARTESIAN_POINT ( 'NONE',  ( 2.351212046067109984, -0.9815930753335269099, 4.597298481426010497 ) ) ;
#13220 = EDGE_CURVE ( 'NONE', #4106, #1517, #10297, .T. ) ;
#13221 = AXIS2_PLACEMENT_3D ( 'NONE', #13843, #1337, #17988 ) ;
#13222 = CARTESIAN_POINT ( 'NONE',  ( -2.224278379903029901, -0.5091101694915259879, 5.468825643806110470 ) ) ;
#13223 = VECTOR ( 'NONE', #14189, 1000.000000000000000 ) ;
#13224 = EDGE_CURVE ( 'NONE', #9615, #13769, #9606, .T. ) ;
#13225 = DIRECTION ( 'NONE',  ( 0.000000000000000000, 0.000000000000000000, 1.000000000000000000 ) ) ;
#13226 = VERTEX_POINT ( 'NONE', #4043 ) ;
#13227 = CARTESIAN_POINT ( 'NONE',  ( 1.899999999999999911, 4.700000000000000178, 1.600000000000000089 ) ) ;
#13228 = VERTEX_POINT ( 'NONE', #1093 ) ;
#13229 = CARTESIAN_POINT ( 'NONE',  ( -1.149999999999999911, 9.299999999999998934, 7.599999999999999645 ) ) ;
#13230 = VECTOR ( 'NONE', #7071, 1000.000000000000000 ) ;
#13231 = CARTESIAN_POINT ( 'NONE',  ( -1.000000000000000000, -6.000000000000000000, 5.100000000000000533 ) ) ;
#13232 = VECTOR ( 'NONE', #12515, 1000.000000000000000 ) ;
#13233 = AXIS2_PLACEMENT_3D ( 'NONE', #2036, #3334, #7873 ) ;
#13234 = EDGE_LOOP ( 'NONE', ( #8231, #1523, #3397, #6327 ) ) ;
#13235 = B_SPLINE_CURVE_WITH_KNOTS ( 'NONE', 3,
 ( #9723, #6764, #1026, #2329, #13625, #13892, #5186 ),
 .UNSPECIFIED., .F., .F.,
 ( 4, 1, 1, 1, 4 ),
 ( 18.06415775814129887, 18.36448856483159986, 18.49670707487869947, 18.62179267666130045, 18.84955592153880133 ),
 .UNSPECIFIED. ) ;
#13236 = CARTESIAN_POINT ( 'NONE',  ( 1.687170344132030042, -2.751502985243429844, 6.340793075730549511 ) ) ;
#13237 = AXIS2_PLACEMENT_3D ( 'NONE', #17893, #6529, #891 ) ;
#13238 = LINE ( 'NONE', #15843, #16174 ) ;
#13239 = DIRECTION ( 'NONE',  ( -1.000000000000000000, 0.000000000000000000, 1.586032892321649771E-16 ) ) ;
#13240 = EDGE_CURVE ( 'NONE', #16121, #14329, #12393, .T. ) ;
#13241 = CARTESIAN_POINT ( 'NONE',  ( 1.571912189623089873, -4.335106588847041031, 6.451524409078630562 ) ) ;
#13242 = VECTOR ( 'NONE', #12407, 1000.000000000000000 ) ;
#13243 = CARTESIAN_POINT ( 'NONE',  ( -1.440522616026439495, -4.804713230972779137, 3.241384813161591438 ) ) ;
#13244 = EDGE_CURVE ( 'NONE', #2833, #12628, #12052, .T. ) ;
#13245 = CARTESIAN_POINT ( 'NONE',  ( 1.149999999999999911, 6.447051294741199534, 6.942609934460510779 ) ) ;
#13246 = PLANE ( 'NONE',  #5010 ) ;
#13247 = AXIS2_PLACEMENT_3D ( 'NONE', #12797, #1596, #7240 ) ;
#13248 = ORIENTED_EDGE ( 'NONE', *, *, #5414, .T. ) ;
#13249 = VECTOR ( 'NONE', #12352, 1000.000000000000000 ) ;
#13250 = CARTESIAN_POINT ( 'NONE',  ( -0.05465110135555984600, -0.1512711864406780515, 6.752241303418941243 ) ) ;
#13251 = CARTESIAN_POINT ( 'NONE',  ( -1.332058588847369940, -3.100827309567760537, 6.640197310420220767 ) ) ;
#13252 = EDGE_LOOP ( 'NONE', ( #17716, #10530, #4606, #17903 ) ) ;
#13253 = ORIENTED_EDGE ( 'NONE', *, *, #13770, .T. ) ;
#13254 = CYLINDRICAL_SURFACE ( 'NONE', #2336, 0.2500000000000002220 ) ;
#13255 = ORIENTED_EDGE ( 'NONE', *, *, #13069, .T. ) ;
#13256 = DIRECTION ( 'NONE',  ( 1.000000000000000000, -8.673617379884035472E-15, 0.000000000000000000 ) ) ;
#13257 = VECTOR ( 'NONE', #7469, 1000.000000000000000 ) ;
#13258 = CARTESIAN_POINT ( 'NONE',  ( -2.484260633728970546, -5.242161016949150820, 3.766563288620799366 ) ) ;
#13259 = CIRCLE ( 'NONE', #6444, 0.2500000000000002220 ) ;
#13260 = CARTESIAN_POINT ( 'NONE',  ( 1.000000000000000000, -7.000000000000000000, 5.700000000000000178 ) ) ;
#13261 = CARTESIAN_POINT ( 'NONE',  ( 1.707817112497189926, -0.4112288135593229477, 6.319218296629480314 ) ) ;
#13262 = ORIENTED_EDGE ( 'NONE', *, *, #6495, .F. ) ;
#13263 = DIRECTION ( 'NONE',  ( 0.000000000000000000, 0.000000000000000000, 1.000000000000000000 ) ) ;
#13264 = EDGE_CURVE ( 'NONE', #13454, #4371, #17973, .T. ) ;
#13265 = CARTESIAN_POINT ( 'NONE',  ( 2.044452488559148851, -4.148800282540726414, 4.887392274793745273 ) ) ;
#13266 = CARTESIAN_POINT ( 'NONE',  ( 0.7322514394120266390, -0.01334745762711889508, 2.149183891723918993 ) ) ;
#13267 = EDGE_CURVE ( 'NONE', #9279, #14793, #2572, .T. ) ;
#13268 = ORIENTED_EDGE ( 'NONE', *, *, #7900, .F. ) ;
#13269 = CARTESIAN_POINT ( 'NONE',  ( 0.6493550500446280127, -0.3133474576271190193, 2.437955526623099889 ) ) ;
#13270 = AXIS2_PLACEMENT_3D ( 'NONE', #2397, #13302, #10713 ) ;
#13271 = VERTEX_POINT ( 'NONE', #18180 ) ;
#13272 = CARTESIAN_POINT ( 'NONE',  ( 1.554165089654128584, -0.4201271186440683758, 6.851145244874527584 ) ) ;
#13273 = ORIENTED_EDGE ( 'NONE', *, *, #16282, .T. ) ;
#13274 = DIRECTION ( 'NONE',  ( 1.000000000000000000, 0.000000000000000000, 0.000000000000000000 ) ) ;
#13275 = DIRECTION ( 'NONE',  ( 1.224646799147350002E-16, -1.000000000000000000, -6.123233995736769734E-17 ) ) ;
#13276 = EDGE_CURVE ( 'NONE', #16395, #1884, #5719, .T. ) ;
#13277 = DIRECTION ( 'NONE',  ( 1.000000000000000000, 1.741945227011179869E-17, 2.220446049250309876E-16 ) ) ;
#13278 = CARTESIAN_POINT ( 'NONE',  ( 0.4469859058769135030, -3.776187669928120272, 2.084026511420788985 ) ) ;
#13279 = VERTEX_POINT ( 'NONE', #8225 ) ;
#13280 = AXIS2_PLACEMENT_3D ( 'NONE', #16961, #4271, #14362 ) ;
#13281 = CARTESIAN_POINT ( 'NONE',  ( 1.948278411993589865, -2.406019537279080467, 6.020210936496000365 ) ) ;
#13282 = DIRECTION ( 'NONE',  ( 4.265713465516724418E-16, 1.000000000000000000, -8.531426931033448836E-16 ) ) ;
#13283 = DIRECTION ( 'NONE',  ( -1.850371707708589879E-16, -1.000000000000000000, 0.000000000000000000 ) ) ;
#13284 = CARTESIAN_POINT ( 'NONE',  ( 0.8735826871841618768, -4.106064582324130185, 6.557889967484662463 ) ) ;
#13285 = DIRECTION ( 'NONE',  ( -0.7071067811865502373, 0.000000000000000000, -0.7071067811865447972 ) ) ;
#13286 = CARTESIAN_POINT ( 'NONE',  ( 1.555285212483259683, -2.079983501243050981, 3.359854578615069087 ) ) ;
#13287 = ORIENTED_EDGE ( 'NONE', *, *, #3008, .F. ) ;
#13288 = CARTESIAN_POINT ( 'NONE',  ( 1.307725206348619995, -0.7471169921413569615, 2.732408283416570161 ) ) ;
#13289 = EDGE_LOOP ( 'NONE', ( #11266, #4050, #8431, #8327 ) ) ;
#13290 = VECTOR ( 'NONE', #11107, 1000.000000000000000 ) ;
#13291 = DIRECTION ( 'NONE',  ( -1.000000000000000000, -2.337311630789800155E-16, -2.220446049250309876E-16 ) ) ;
#13292 = DIRECTION ( 'NONE',  ( 0.000000000000000000, -1.000000000000000000, 0.000000000000000000 ) ) ;
#13293 = LINE ( 'NONE', #4497, #15696 ) ;
#13294 = EDGE_CURVE ( 'NONE', #2455, #10006, #13957, .T. ) ;
#13295 = CARTESIAN_POINT ( 'NONE',  ( 1.300961508564179914, -5.122033898305089927, 6.661123742937279602 ) ) ;
#13296 = ORIENTED_EDGE ( 'NONE', *, *, #3141, .F. ) ;
#13297 = VERTEX_POINT ( 'NONE', #2668 ) ;
#13298 = DIRECTION ( 'NONE',  ( 0.000000000000000000, -0.2588190451025180749, 0.9659258262890690894 ) ) ;
#13299 = CARTESIAN_POINT ( 'NONE',  ( 1.399999999999999911, -8.000000000000000000, 6.100000000000000533 ) ) ;
#13300 = CARTESIAN_POINT ( 'NONE',  ( 1.652654650382400003, -0.7952867690272209522, 3.029252778805629820 ) ) ;
#13301 = ORIENTED_EDGE ( 'NONE', *, *, #2590, .T. ) ;
#13302 = DIRECTION ( 'NONE',  ( -1.224646799147350002E-16, 1.000000000000000000, 6.123233995736759873E-17 ) ) ;
#13303 = CARTESIAN_POINT ( 'NONE',  ( -0.4722227023514615762, -2.122719201459649874, 2.088464165977090836 ) ) ;
#13304 = PRODUCT_DEFINITION ( 'UNKNOWN', '', #7383, #8262 ) ;
#13305 = DIRECTION ( 'NONE',  ( 0.000000000000000000, -5.224578939412490694E-16, 1.000000000000000000 ) ) ;
#13306 = CARTESIAN_POINT ( 'NONE',  ( 0.6914213562373089372, 3.050000000000000266, 2.557842712474620139 ) ) ;
#13307 = EDGE_CURVE ( 'NONE', #17501, #15103, #16220, .T. ) ;
#13308 = AXIS2_PLACEMENT_3D ( 'NONE', #1814, #12915, #143 ) ;
#13309 = CARTESIAN_POINT ( 'NONE',  ( -2.126557263589650137, -3.151244762504310071, 3.691783806836059778 ) ) ;
#13310 = CARTESIAN_POINT ( 'NONE',  ( 0.1969988207263408952, -5.304612347394259686, 2.648915996644538584 ) ) ;
#13311 = CARTESIAN_POINT ( 'NONE',  ( 2.516451517878131927, -0.9117282104686613708, 3.857037693030633818 ) ) ;
#13312 = DIRECTION ( 'NONE',  ( -1.000000000000000000, 0.000000000000000000, 0.000000000000000000 ) ) ;
#13313 = CARTESIAN_POINT ( 'NONE',  ( 1.899999999999999911, 0.7500000000000000000, 7.649999999999999467 ) ) ;
#13314 = CARTESIAN_POINT ( 'NONE',  ( 1.851400890972779045, -5.413135593220339992, 6.601359968904126241 ) ) ;
#13315 = VERTEX_POINT ( 'NONE', #1187 ) ;
#13316 = CARTESIAN_POINT ( 'NONE',  ( 1.661700935788380074, -5.337500000000000355, 3.038299064211610112 ) ) ;
#13317 = ORIENTED_EDGE ( 'NONE', *, *, #1873, .T. ) ;
#13318 = EDGE_CURVE ( 'NONE', #17967, #2437, #11002, .T. ) ;
#13319 = LINE ( 'NONE', #635, #9378 ) ;
#13320 = VECTOR ( 'NONE', #11548, 1000.000000000000000 ) ;
#13321 = CARTESIAN_POINT ( 'NONE',  ( -4.898587196589392737E-17, 5.318248954186070243, 6.349999999999999645 ) ) ;
#13322 = EDGE_CURVE ( 'NONE', #786, #6313, #11084, .T. ) ;
#13323 = ORIENTED_EDGE ( 'NONE', *, *, #5645, .T. ) ;
#13324 = ADVANCED_FACE ( 'NONE', ( #4137 ), #11365, .T. ) ;
#13325 = CARTESIAN_POINT ( 'NONE',  ( 2.023259452208809872, -2.425466949207399914, 3.497849062500220096 ) ) ;
#13326 = EDGE_CURVE ( 'NONE', #1947, #16854, #15455, .T. ) ;
#13327 = CARTESIAN_POINT ( 'NONE',  ( 1.899999999999999911, 6.661338147750959950E-17, 9.955530934770520091 ) ) ;
#13328 = LINE ( 'NONE', #10179, #14403 ) ;
#13329 = EDGE_CURVE ( 'NONE', #16159, #13183, #8408, .T. ) ;
#13330 = DIRECTION ( 'NONE',  ( 1.224646799147350002E-16, -1.000000000000000000, -6.123233995736769734E-17 ) ) ;
#13331 = ADVANCED_FACE ( 'NONE', ( #1465 ), #12761, .T. ) ;
#13332 = CARTESIAN_POINT ( 'NONE',  ( -1.197297565406129971, -1.517223705964160008, 6.726135293448209929 ) ) ;
#13333 = VECTOR ( 'NONE', #16499, 1000.000000000000000 ) ;
#13334 = CARTESIAN_POINT ( 'NONE',  ( -0.4790341583531910197, -3.683034516774959855, 2.395814251711740006 ) ) ;
#13335 = CARTESIAN_POINT ( 'NONE',  ( -1.996236309555629251, -4.548542059801595094, 5.179523137126564869 ) ) ;
#13336 = LINE ( 'NONE', #13427, #2621 ) ;
#13337 = CARTESIAN_POINT ( 'NONE',  ( -1.494593880360799432, -0.5610169491525425212, 3.295456077495951153 ) ) ;
#13338 = DIRECTION ( 'NONE',  ( -0.000000000000000000, 1.000000000000000000, 0.000000000000000000 ) ) ;
#13339 = VERTEX_POINT ( 'NONE', #5983 ) ;
#13340 = DIRECTION ( 'NONE',  ( -1.000000000000000000, 0.000000000000000000, 1.586032892321649771E-16 ) ) ;
#13341 = CARTESIAN_POINT ( 'NONE',  ( 1.821706171509118954, -0.09788135593220394226, 5.646608543709396244 ) ) ;
#13342 = CARTESIAN_POINT ( 'NONE',  ( -2.036228139452650243, -3.473439922180369788, 3.519948877554409883 ) ) ;
#13343 = ORIENTED_EDGE ( 'NONE', *, *, #8924, .F. ) ;
#13344 = EDGE_LOOP ( 'NONE', ( #11568, #13824, #9273, #2243 ) ) ;
#13345 = CARTESIAN_POINT ( 'NONE',  ( -1.408343819019460219E-16, 2.299999999999999822, 5.100000000000000533 ) ) ;
#13346 = EDGE_LOOP ( 'NONE', ( #167, #1824, #7597, #17622 ) ) ;
#13347 = CARTESIAN_POINT ( 'NONE',  ( -1.889999999999999902, 3.500000000000000000, 0.5999999999999999778 ) ) ;
#13348 = ITEM_DEFINED_TRANSFORMATION ( 'NONE', 'NONE', #15364,  #17681 ) ;
#13349 = CARTESIAN_POINT ( 'NONE',  ( -1.407651048079459288, -5.273305084745764759, 2.450250343405070641 ) ) ;
#13350 = EDGE_CURVE ( 'NONE', #17115, #4659, #8761, .T. ) ;
#13351 = CARTESIAN_POINT ( 'NONE',  ( 1.850000000000000089, -6.000000000000000000, 2.799999999999999822 ) ) ;
#13352 = CARTESIAN_POINT ( 'NONE',  ( -1.791574935211209807, -0.4913135593220339659, 6.226029630577610163 ) ) ;
#13353 = EDGE_LOOP ( 'NONE', ( #17515, #55, #15852, #14997 ) ) ;
#13354 = LINE ( 'NONE', #16666, #1086 ) ;
#13355 = CARTESIAN_POINT ( 'NONE',  ( 0.5381211601353905749, -4.451548030288480895, 6.681243917250638376 ) ) ;
#13356 = CARTESIAN_POINT ( 'NONE',  ( 0.9002849211310119948, -0.4334745762711874617, 7.196465912290821443 ) ) ;
#13357 = VERTEX_POINT ( 'NONE', #17087 ) ;
#13358 = CARTESIAN_POINT ( 'NONE',  ( -1.679950111053631900, -0.4957627118644069575, 5.880020650119711867 ) ) ;
#13359 = ADVANCED_FACE ( 'NONE', ( #5897, #8857 ), #17173, .T. ) ;
#13360 = CARTESIAN_POINT ( 'NONE',  ( -2.651721837666119796, -0.5269067796610176213, 4.594045830208265180 ) ) ;
#13361 = ORIENTED_EDGE ( 'NONE', *, *, #5518, .F. ) ;
#13362 = CARTESIAN_POINT ( 'NONE',  ( -1.800000000000000044, 12.00000000000000000, 7.649999999999999467 ) ) ;
#13363 = AXIS2_PLACEMENT_3D ( 'NONE', #1113, #13789, #7041 ) ;
#13364 = CARTESIAN_POINT ( 'NONE',  ( 0.8934014991060327260, -0.9854339516935011201, 6.877287176483389608 ) ) ;
#13365 = CARTESIAN_POINT ( 'NONE',  ( -1.303682947472720954, -0.2673043920988010802, 3.104350467804975366 ) ) ;
#13366 = CARTESIAN_POINT ( 'NONE',  ( -1.650842931266140790, -3.566593075333521767, 2.622060802311461547 ) ) ;
#13367 = EDGE_CURVE ( 'NONE', #4524, #6834, #4413, .T. ) ;
#13368 = VERTEX_POINT ( 'NONE', #7386 ) ;
#13369 = CARTESIAN_POINT ( 'NONE',  ( 0.7435598031058590074, -2.569037555297100095, 6.932904947974519949 ) ) ;
#13370 = DIRECTION ( 'NONE',  ( 1.850371707708589879E-16, 1.000000000000000000, -9.251858538542959255E-17 ) ) ;
#13371 = CARTESIAN_POINT ( 'NONE',  ( 1.889999999999999902, 8.500000000000000000, 4.204760881734880211E-16 ) ) ;
#13372 = CARTESIAN_POINT ( 'NONE',  ( -1.102492180652080211, -3.290974492234041815, 2.968118700883599193 ) ) ;
#13373 = DIRECTION ( 'NONE',  ( 1.000000000000000000, 0.000000000000000000, 0.000000000000000000 ) ) ;
#13374 = CARTESIAN_POINT ( 'NONE',  ( -1.750000000000000000, 11.40000000000000036, 7.700000000000000178 ) ) ;
#13375 = CARTESIAN_POINT ( 'NONE',  ( -1.508881462028629716, -1.288181699441250050, 6.092184821126286565 ) ) ;
#13376 = ORIENTED_EDGE ( 'NONE', *, *, #13452, .F. ) ;
#13377 = DIRECTION ( 'NONE',  ( 2.775557561562900226E-16, 1.000000000000000000, -2.775557561562900226E-16 ) ) ;
#13378 = FACE_BOUND ( 'NONE', #1562, .T. ) ;
#13379 = CARTESIAN_POINT ( 'NONE',  ( -0.9279264017968105183, -1.171740257999810852, 7.186376135231811624 ) ) ;
#13380 = VECTOR ( 'NONE', #9325, 1000.000000000000000 ) ;
#13381 = ORIENTED_EDGE ( 'NONE', *, *, #761, .F. ) ;
#13382 = LINE ( 'NONE', #9206, #4340 ) ;
#13383 = CARTESIAN_POINT ( 'NONE',  ( -1.000000000000000000, -5.599999999999999645, 3.673738709727309981 ) ) ;
#13384 = DIRECTION ( 'NONE',  ( 0.000000000000000000, 0.000000000000000000, -1.000000000000000000 ) ) ;
#13385 = CARTESIAN_POINT ( 'NONE',  ( -0.07299321914061848715, -5.298516949152539901, 2.350000000000000089 ) ) ;
#13386 = ORIENTED_EDGE ( 'NONE', *, *, #1332, .F. ) ;
#13387 =( BOUNDED_SURFACE ( )  B_SPLINE_SURFACE ( 3, 3, ( 
 ( #11644, #11741, #13041, #9035, #3227, #17270, #10349 ),
 ( #8959, #15742, #7486, #11558, #15916, #6087, #17462 ),
 ( #7665, #1755, #2008, #3316, #446, #8690, #1655 ),
 ( #17542, #626, #17374, #4696, #16015, #14604, #12951 ),
 ( #1919, #7304, #7569, #13215, #4782, #10432, #16094 ),
 ( #3390, #13310, #6264, #14692, #4871, #277, #4512 ),
 ( #10163, #15823, #3126, #10518, #9226, #9519, #6452 ) ),
 .UNSPECIFIED., .T., .F., .F. ) 
 B_SPLINE_SURFACE_WITH_KNOTS ( ( 4, 3, 4 ),
 ( 4, 1, 1, 1, 4 ),
 ( 0.000000000000000000, 3.141592653589790007, 6.283185307179590673 ),
 ( 0.000000000000000000, 0.3003308066894049833, 0.4325493167363730351, 0.5576349185191149527, 0.7853981633974479459 ),
 .UNSPECIFIED. ) 
 GEOMETRIC_REPRESENTATION_ITEM ( )  RATIONAL_B_SPLINE_SURFACE ( (
 ( 1.000000000000000000, 1.000000000000000000, 1.000000000000000000, 1.000000000000000000, 1.000000000000000000, 1.000000000000000000, 1.000000000000000000),
 ( 0.3333333333333329818, 0.3333333333333329818, 0.3333333333333329818, 0.3333333333333329818, 0.3333333333333329818, 0.3333333333333329818, 0.3333333333333329818),
 ( 0.3333333333333329818, 0.3333333333333329818, 0.3333333333333329818, 0.3333333333333329818, 0.3333333333333329818, 0.3333333333333329818, 0.3333333333333329818),
 ( 1.000000000000000000, 1.000000000000000000, 1.000000000000000000, 1.000000000000000000, 1.000000000000000000, 1.000000000000000000, 1.000000000000000000),
 ( 0.3333333333333329818, 0.3333333333333329818, 0.3333333333333329818, 0.3333333333333329818, 0.3333333333333329818, 0.3333333333333329818, 0.3333333333333329818),
 ( 0.3333333333333329818, 0.3333333333333329818, 0.3333333333333329818, 0.3333333333333329818, 0.3333333333333329818, 0.3333333333333329818, 0.3333333333333329818),
 ( 1.000000000000000000, 1.000000000000000000, 1.000000000000000000, 1.000000000000000000, 1.000000000000000000, 1.000000000000000000, 1.000000000000000000) ) ) 
 REPRESENTATION_ITEM ( '' )  SURFACE ( )  );
#13388 = ORIENTED_EDGE ( 'NONE', *, *, #15041, .F. ) ;
#13389 = CARTESIAN_POINT ( 'NONE',  ( 2.500000000000000000, 2.799999999999999822, 1.600000000000000089 ) ) ;
#13390 = DIRECTION ( 'NONE',  ( -1.000000000000000000, 4.743384504624081899E-16, 0.000000000000000000 ) ) ;
#13391 = CARTESIAN_POINT ( 'NONE',  ( 1.899999999999999911, 2.481229107598850043E-16, 7.649999999999999467 ) ) ;
#13392 = ORIENTED_EDGE ( 'NONE', *, *, #7104, .F. ) ;
#13393 = CARTESIAN_POINT ( 'NONE',  ( -1.901882987994748975, -5.506567796610171150, 5.472995608211450147 ) ) ;
#13394 = CARTESIAN_POINT ( 'NONE',  ( -2.647661051184980519, -3.058091609351150986, 4.518328177639144627 ) ) ;
#13395 = DIRECTION ( 'NONE',  ( 1.000000000000000000, -1.054711873393900133E-14, 1.850371707708589879E-16 ) ) ;
#13396 = CARTESIAN_POINT ( 'NONE',  ( 2.146130664537611032, -2.402178660919109365, 3.138834773724044958 ) ) ;
#13397 = DIRECTION ( 'NONE',  ( 0.000000000000000000, -1.000000000000000000, -1.332267629550190018E-15 ) ) ;
#13398 = CYLINDRICAL_SURFACE ( 'NONE', #17940, 0.2500000000000002220 ) ;
#13399 = CARTESIAN_POINT ( 'NONE',  ( 1.197297565406180153, -4.082776294035840969, 6.726135293448179731 ) ) ;
#13400 = CARTESIAN_POINT ( 'NONE',  ( 1.889999999999999902, 7.900000000000000355, 0.5999999999999999778 ) ) ;
#13401 = LINE ( 'NONE', #1776, #18280 ) ;
#13403 = ORIENTED_EDGE ( 'NONE', *, *, #7449, .T. ) ;
#13402 = CARTESIAN_POINT ( 'NONE',  ( 1.630703155447489561, -2.332313796054251487, 2.606218513833050920 ) ) ;
#13404 = CARTESIAN_POINT ( 'NONE',  ( 0.2000000000000000111, -2.449293598294700066E-17, 8.300000000000000711 ) ) ;
#13405 = CARTESIAN_POINT ( 'NONE',  ( -1.000000000000000000, -7.000000000000000000, 5.700000000000000178 ) ) ;
#13406 = CARTESIAN_POINT ( 'NONE',  ( 1.661700935665417544, -5.037501140877957084, 3.038299064334577082 ) ) ;
#13407 = DIRECTION ( 'NONE',  ( 1.000000000000000000, 1.306144734853129823E-16, 0.000000000000000000 ) ) ;
#13408 = CARTESIAN_POINT ( 'NONE',  ( -0.4201920264140019956, -2.122719201459649874, 2.384360920086639801 ) ) ;
#13409 = LINE ( 'NONE', #9438, #4429 ) ;
#13410 = CARTESIAN_POINT ( 'NONE',  ( -2.340070819011249803, -5.519915254237290014, 4.950151441910549899 ) ) ;
#13411 = ORIENTED_EDGE ( 'NONE', *, *, #2125, .F. ) ;
#13412 = DIRECTION ( 'NONE',  ( -1.224646799147350002E-16, 8.383884571949770538E-16, -1.000000000000000000 ) ) ;
#13413 = VERTEX_POINT ( 'NONE', #14505 ) ;
#13414 = LINE ( 'NONE', #727, #7013 ) ;
#13415 = DIRECTION ( 'NONE',  ( 1.000000000000000000, -1.224646799147350002E-16, 0.000000000000000000 ) ) ;
#13416 = ORIENTED_EDGE ( 'NONE', *, *, #7216, .T. ) ;
#13417 = VERTEX_POINT ( 'NONE', #7548 ) ;
#13418 = CARTESIAN_POINT ( 'NONE',  ( -1.586727176531439909, -1.982989471729919906, 2.961885344765640138 ) ) ;
#13419 = FACE_OUTER_BOUND ( 'NONE', #16525, .T. ) ;
#13420 = CARTESIAN_POINT ( 'NONE',  ( -1.378221871957430178, -5.479872881355929870, 6.607619368096279366 ) ) ;
#13421 = VECTOR ( 'NONE', #11482, 1000.000000000000000 ) ;
#13422 = DIRECTION ( 'NONE',  ( 1.000000000000000000, 0.000000000000000000, 0.000000000000000000 ) ) ;
#13423 = CARTESIAN_POINT ( 'NONE',  ( -1.750000000000000000, 0.5999999999999999778, 7.700000000000000178 ) ) ;
#13424 = CARTESIAN_POINT ( 'NONE',  ( 2.342931736853870017, -4.102223705964150646, 4.477701633099130163 ) ) ;
#13425 = CARTESIAN_POINT ( 'NONE',  ( 2.039016451601951108, -2.588484967225421762, 4.939402908764060740 ) ) ;
#13426 = EDGE_CURVE ( 'NONE', #16693, #16922, #10072, .T. ) ;
#13427 = CARTESIAN_POINT ( 'NONE',  ( 1.899999999999999911, 9.199999999999999289, 1.600000000000000089 ) ) ;
#13428 = B_SPLINE_CURVE_WITH_KNOTS ( 'NONE', 3,
 ( #454, #6361, #6095, #11754, #16102, #7675, #13316 ),
 .UNSPECIFIED., .F., .F.,
 ( 4, 1, 1, 1, 4 ),
 ( 0.000000000000000000, 0.3003308066894049833, 0.4325493167363730351, 0.5576349185191149527, 0.7853981633974479459 ),
 .UNSPECIFIED. ) ;
#13429 = CARTESIAN_POINT ( 'NONE',  ( 1.875000000000000000, 0.7500000000000000000, 8.300000000000000711 ) ) ;
#13430 = ORIENTED_EDGE ( 'NONE', *, *, #14397, .F. ) ;
#13431 = EDGE_CURVE ( 'NONE', #12376, #3539, #17349, .T. ) ;
#13432 = CARTESIAN_POINT ( 'NONE',  ( 0.9000000000000000222, 6.450000000000000178, 1.600000000000000089 ) ) ;
#13433 = CARTESIAN_POINT ( 'NONE',  ( -1.286937324407759986, -3.589881363621809651, 2.729584305145209999 ) ) ;
#13434 = COLOUR_RGB ( '', 0.31764706, 0.68627451, 0.89019608) ;
#13435 = VERTEX_POINT ( 'NONE', #12843 ) ;
#13436 = EDGE_CURVE ( 'NONE', #3824, #2153, #7286, .T. ) ;
#13437 = ORIENTED_EDGE ( 'NONE', *, *, #320, .F. ) ;
#13438 = ADVANCED_FACE ( 'NONE', ( #17254 ), #8670, .F. ) ;
#13439 = DIRECTION ( 'NONE',  ( 1.224646799147350002E-16, -1.000000000000000000, -6.123233995736769734E-17 ) ) ;
#13440 = ORIENTED_EDGE ( 'NONE', *, *, #8682, .T. ) ;
#13441 = LINE ( 'NONE', #10850, #13333 ) ;
#13442 = PRODUCT_CONTEXT ( 'NONE', #14650, 'mechanical' ) ;
#13443 = CARTESIAN_POINT ( 'NONE',  ( 2.224278379903029901, -5.090889830508480429, 5.468825643806100700 ) ) ;
#13444 = FACE_OUTER_BOUND ( 'NONE', #15074, .T. ) ;
#13445 = ORIENTED_EDGE ( 'NONE', *, *, #6228, .F. ) ;
#13446 = DIRECTION ( 'NONE',  ( 4.440892098500630106E-16, 0.000000000000000000, -1.000000000000000000 ) ) ;
#13447 = CARTESIAN_POINT ( 'NONE',  ( 0.1608173401625761778, -4.498124606865046893, 6.746714348835997299 ) ) ;
#13448 = CARTESIAN_POINT ( 'NONE',  ( 0.6640878839024751956, -0.4379237288135597317, 7.269405042592523181 ) ) ;
#13449 = VERTEX_POINT ( 'NONE', #11625 ) ;
#13450 = CARTESIAN_POINT ( 'NONE',  ( 0.4360591020457930123, -0.3088983050847460277, 2.387347919655840034 ) ) ;
#13451 = EDGE_LOOP ( 'NONE', ( #1319, #3455, #9414, #13741 ) ) ;
#13452 = EDGE_CURVE ( 'NONE', #10145, #4379, #13024, .T. ) ;
#13453 = CARTESIAN_POINT ( 'NONE',  ( -1.851400890972779045, -0.1868644067796610686, 6.601359968904141340 ) ) ;
#13454 = VERTEX_POINT ( 'NONE', #261 ) ;
#13455 = CARTESIAN_POINT ( 'NONE',  ( 0.03714311608463249925, -1.078587104846650435, 7.053160869216426931 ) ) ;
#13456 = CARTESIAN_POINT ( 'NONE',  ( -0.1869574461324000070, -0.5962015548080630278, 2.350675676344399889 ) ) ;
#13457 = CARTESIAN_POINT ( 'NONE',  ( -2.199635523370571111, -5.057043525783965876, 3.215170965529011493 ) ) ;
#13458 = ORIENTED_EDGE ( 'NONE', *, *, #17578, .F. ) ;
#13459 = LINE ( 'NONE', #776, #3699 ) ;
#13460 = CARTESIAN_POINT ( 'NONE',  ( -1.265407828724339989, -3.290974492234040483, 2.715689360385570073 ) ) ;
#13461 = CARTESIAN_POINT ( 'NONE',  ( -0.7756407636288503715, -4.591277760018214416, 7.238010066725332869 ) ) ;
#13462 = DIRECTION ( 'NONE',  ( 5.872254014546280719E-16, -5.872254014546280719E-16, 1.000000000000000000 ) ) ;
#13463 = CARTESIAN_POINT ( 'NONE',  ( -11.62823001646920140, -8.079925217494299891E-16, -2.930988785010409480E-14 ) ) ;
#13464 = CARTESIAN_POINT ( 'NONE',  ( -0.4365326870213908639, -4.269082600342137823, 6.706076034398992469 ) ) ;
#13465 = DIRECTION ( 'NONE',  ( 5.296209390990920866E-31, 1.000000000000000000, 8.548717289613711672E-15 ) ) ;
#13466 = PLANE ( 'NONE',  #17688 ) ;
#13467 = CARTESIAN_POINT ( 'NONE',  ( -1.217499609005920025, -1.707370888630439065, 3.046943272389440960 ) ) ;
#13468 = VERTEX_POINT ( 'NONE', #4493 ) ;
#13469 = CARTESIAN_POINT ( 'NONE',  ( -0.1749999999999999889, 7.900000000000000355, 0.4000000000000000222 ) ) ;
#13470 =( REPRESENTATION_RELATIONSHIP ('NONE','NONE', #2757, #853 ) REPRESENTATION_RELATIONSHIP_WITH_TRANSFORMATION ( #4815 )SHAPE_REPRESENTATION_RELATIONSHIP( ) );
#13471 = EDGE_CURVE ( 'NONE', #3917, #4727, #15802, .T. ) ;
#13472 = CARTESIAN_POINT ( 'NONE',  ( 0.5637478356992829953, -0.6606104644819250638, 2.398845082743519708 ) ) ;
#13473 = CARTESIAN_POINT ( 'NONE',  ( 1.292937800126339631, -2.522460978720530989, 7.017633607369027082 ) ) ;
#13474 = ORIENTED_EDGE ( 'NONE', *, *, #14335, .T. ) ;
#13475 = DIRECTION ( 'NONE',  ( -0.7071067811865500152, 0.000000000000000000, -0.7071067811865451302 ) ) ;
#13476 = CARTESIAN_POINT ( 'NONE',  ( 2.046174187462399985, -1.121322805063259986, 5.862719605943959245 ) ) ;
#13477 = DIRECTION ( 'NONE',  ( 0.000000000000000000, 0.000000000000000000, 1.000000000000000000 ) ) ;
#13478 = CARTESIAN_POINT ( 'NONE',  ( 0.06264882350516240428, -5.148728813559320550, 7.052569299041220319 ) ) ;
#13479 = ORIENTED_EDGE ( 'NONE', *, *, #4617, .F. ) ;
#13480 = ORIENTED_EDGE ( 'NONE', *, *, #12243, .T. ) ;
#13481 = LINE ( 'NONE', #9508, #8008 ) ;
#13482 = DIRECTION ( 'NONE',  ( 2.055968564120659776E-16, 1.000000000000000000, 0.000000000000000000 ) ) ;
#13483 = DIRECTION ( 'NONE',  ( 0.000000000000000000, 0.000000000000000000, 1.000000000000000000 ) ) ;
#13484 = ORIENTED_EDGE ( 'NONE', *, *, #12436, .F. ) ;
#13485 = AXIS2_PLACEMENT_3D ( 'NONE', #4053, #9708, #8233 ) ;
#13486 = CARTESIAN_POINT ( 'NONE',  ( -0.9222751404131109831, -5.577754237288145234, 2.865854510788139908 ) ) ;
#13487 = CARTESIAN_POINT ( 'NONE',  ( 1.788074174585509768, -3.617010528270069525, 2.738902236199779239 ) ) ;
#13488 = CARTESIAN_POINT ( 'NONE',  ( 1.271629043573289915E-13, 12.00000000000000000, -5.003920418925160367E-17 ) ) ;
#13489 = CARTESIAN_POINT ( 'NONE',  ( -1.292937800126279679, -3.077539021279473097, 7.017633607369056392 ) ) ;
#13490 = AXIS2_PLACEMENT_3D ( 'NONE', #15665, #8694, #10092 ) ;
#13491 = AXIS2_PLACEMENT_3D ( 'NONE', #10996, #5440, #11170 ) ;
#13492 = DIRECTION ( 'NONE',  ( 0.000000000000000000, 0.000000000000000000, 1.000000000000000000 ) ) ;
#13493 = CYLINDRICAL_SURFACE ( 'NONE', #15906, 0.5999999999999999778 ) ;
#13494 = VECTOR ( 'NONE', #7586, 1000.000000000000000 ) ;
#13495 = CARTESIAN_POINT ( 'NONE',  ( -1.303621121494419999, -4.362235753495300905, 6.659417683669699883 ) ) ;
#13496 = LINE ( 'NONE', #13767, #1695 ) ;
#13497 = DIRECTION ( 'NONE',  ( -1.000000000000000000, 0.000000000000000000, 6.123233995736769734E-17 ) ) ;
#13499 = ORIENTED_EDGE ( 'NONE', *, *, #12562, .T. ) ;
#13498 = CARTESIAN_POINT ( 'NONE',  ( -1.883442729065680776, -3.147403886144331420, 6.569694408006696129 ) ) ;
#13500 = EDGE_CURVE ( 'NONE', #305, #5195, #15994, .T. ) ;
#13501 = PLANE ( 'NONE',  #4673 ) ;
#13502 = DIRECTION ( 'NONE',  ( -1.306144734853129823E-16, 1.000000000000000000, 0.000000000000000000 ) ) ;
#13503 = CARTESIAN_POINT ( 'NONE',  ( -0.1569242594330230167, -1.400782264522720144, 7.048216443236290374 ) ) ;
#13504 = CARTESIAN_POINT ( 'NONE',  ( -1.943632316591239917, -0.5536016949152539057, 3.373048379518170048 ) ) ;
#13505 = CARTESIAN_POINT ( 'NONE',  ( -0.3042893218813459977, 6.450000000000000178, 2.170710678118660031 ) ) ;
#13506 = CARTESIAN_POINT ( 'NONE',  ( -3.408368997776849933E-15, -5.599999999999999645, 2.350000000000000089 ) ) ;
#13507 = EDGE_LOOP ( 'NONE', ( #12066, #5982, #9605, #13702 ) ) ;
#13508 = VECTOR ( 'NONE', #9859, 1000.000000000000000 ) ;
#13509 = LINE ( 'NONE', #1850, #7526 ) ;
#13510 = CARTESIAN_POINT ( 'NONE',  ( 1.000000000000000000, -5.000000000000000000, 3.299999999999999822 ) ) ;
#13511 = DIRECTION ( 'NONE',  ( 7.006492321624090022E-46, 1.000000000000000000, 1.332267629550190018E-15 ) ) ;
#13512 = VECTOR ( 'NONE', #6012, 1000.000000000000000 ) ;
#13513 = ORIENTED_EDGE ( 'NONE', *, *, #2746, .T. ) ;
#13514 = VECTOR ( 'NONE', #6355, 1000.000000000000000 ) ;
#13515 = VECTOR ( 'NONE', #2193, 1000.000000000000000 ) ;
#13516 = ORIENTED_EDGE ( 'NONE', *, *, #12799, .F. ) ;
#13517 = CARTESIAN_POINT ( 'NONE',  ( -2.199335452462570117, -1.866548030288480042, 3.862342996790939953 ) ) ;
#13518 = CARTESIAN_POINT ( 'NONE',  ( -2.180207327701300102, -5.506567796610169374, 5.586116916730199833 ) ) ;
#13519 = AXIS2_PLACEMENT_3D ( 'NONE', #8422, #5737, #17015 ) ;
#13520 = CARTESIAN_POINT ( 'NONE',  ( 2.169623098572349917, -2.658349832090280529, 5.611855963200990338 ) ) ;
#13521 = CIRCLE ( 'NONE', #13209, 0.4000000000000000222 ) ;
#13522 = DIRECTION ( 'NONE',  ( 0.000000000000000000, -1.000000000000000000, -1.959217102279674889E-16 ) ) ;
#13523 = AXIS2_PLACEMENT_3D ( 'NONE', #2386, #2469, #13475 ) ;
#13524 = CARTESIAN_POINT ( 'NONE',  ( -0.1352600594605981310, -1.400782264522720366, 6.748562071049556188 ) ) ;
#13525 = LINE ( 'NONE', #2333, #4947 ) ;
#13526 = CARTESIAN_POINT ( 'NONE',  ( -1.800000000000000044, 11.29999999999999893, 7.649999999999999467 ) ) ;
#13527 = EDGE_LOOP ( 'NONE', ( #15415, #17184, #5006, #3682 ) ) ;
#13528 = LINE ( 'NONE', #2039, #5277 ) ;
#13529 = VECTOR ( 'NONE', #7446, 1000.000000000000000 ) ;
#13530 = DIRECTION ( 'NONE',  ( -1.000000000000000000, 0.000000000000000000, 0.000000000000000000 ) ) ;
#13531 = CARTESIAN_POINT ( 'NONE',  ( -2.219956784870669608, -3.426863345603790023, 3.918630970161619764 ) ) ;
#13532 = ORIENTED_EDGE ( 'NONE', *, *, #322, .F. ) ;
#13533 = ORIENTED_EDGE ( 'NONE', *, *, #7336, .F. ) ;
#13534 = AXIS2_PLACEMENT_3D ( 'NONE', #3204, #14405, #13114 ) ;
#13535 = ORIENTED_EDGE ( 'NONE', *, *, #11077, .T. ) ;
#13536 = VECTOR ( 'NONE', #1820, 1000.000000000000000 ) ;
#13537 = DIRECTION ( 'NONE',  ( 1.000000000000000000, 0.000000000000000000, 0.000000000000000000 ) ) ;
#13538 = ITEM_DEFINED_TRANSFORMATION ( 'NONE', 'NONE', #16224,  #17681 ) ;
#13539 = CARTESIAN_POINT ( 'NONE',  ( -2.345900685764729765, -5.228813559322030180, 4.512231114381339836 ) ) ;
#13540 = STYLED_ITEM ( 'NONE', ( #12495 ), #7985 ) ;
#13541 = ORIENTED_EDGE ( 'NONE', *, *, #5918, .F. ) ;
#13542 = CARTESIAN_POINT ( 'NONE',  ( -2.102728310581289950, -1.358046564306109927, 5.757014351541099195 ) ) ;
#13543 = EDGE_CURVE ( 'NONE', #6171, #10426, #8940, .T. ) ;
#13544 = AXIS2_PLACEMENT_3D ( 'NONE', #6858, #5188, #18118 ) ;
#13545 = CARTESIAN_POINT ( 'NONE',  ( 2.500000000000000000, 7.299999999999999822, 0.5999999999999999778 ) ) ;
#13546 = CARTESIAN_POINT ( 'NONE',  ( 1.627161714697888728, -3.962493976234419790, 3.448102801005814122 ) ) ;
#13547 = CARTESIAN_POINT ( 'NONE',  ( -2.304156201936080617, -0.2002118644067801267, 6.016707707703351282 ) ) ;
#13548 = AXIS2_PLACEMENT_3D ( 'NONE', #7187, #8571, #2650 ) ;
#13549 = ORIENTED_EDGE ( 'NONE', *, *, #16891, .T. ) ;
#13550 = VECTOR ( 'NONE', #10540, 1000.000000000000000 ) ;
#13551 = CARTESIAN_POINT ( 'NONE',  ( -2.625437065641401446, -0.2180084745762719822, 5.087214675345155257 ) ) ;
#13552 = ORIENTED_EDGE ( 'NONE', *, *, #14944, .F. ) ;
#13553 = VECTOR ( 'NONE', #12123, 1000.000000000000000 ) ;
#13554 = VECTOR ( 'NONE', #8532, 1000.000000000000000 ) ;
#13555 = CARTESIAN_POINT ( 'NONE',  ( -1.899999999999999911, 7.299999999999999822, 1.600000000000000089 ) ) ;
#13556 = CARTESIAN_POINT ( 'NONE',  ( -2.345900685764729765, -5.528813559322030002, 4.512231114381339836 ) ) ;
#13557 = CARTESIAN_POINT ( 'NONE',  ( 2.349129089426440054, -0.7059744922340410733, 4.842612091679071362 ) ) ;
#13558 = CARTESIAN_POINT ( 'NONE',  ( 1.641808337277750107, -5.413135593220339103, 6.386111670537619744 ) ) ;
#13559 = CARTESIAN_POINT ( 'NONE',  ( -2.006003143955999324, -4.731007489747939054, 6.437545705712661714 ) ) ;
#13560 = EDGE_LOOP ( 'NONE', ( #5966, #4056, #13248, #14105 ) ) ;
#13561 = VECTOR ( 'NONE', #7882, 1000.000000000000000 ) ;
#13562 = EDGE_CURVE ( 'NONE', #12680, #8572, #3208, .T. ) ;
#13563 = CARTESIAN_POINT ( 'NONE',  ( -0.7046366965007886396, -4.911779243796845051, 2.768871435390180213 ) ) ;
#13564 = CARTESIAN_POINT ( 'NONE',  ( -2.145694642186069867, -4.501965483225029985, 5.666819626392589626 ) ) ;
#13565 = CARTESIAN_POINT ( 'NONE',  ( -2.051568858000911266, -5.080331814072260421, 3.016498023208352919 ) ) ;
#13566 = EDGE_CURVE ( 'NONE', #8965, #6891, #16075, .T. ) ;
#13567 = CARTESIAN_POINT ( 'NONE',  ( 4.898587196589409994E-17, 0.1000000000000000056, 8.300000000000000711 ) ) ;
#13568 = EDGE_CURVE ( 'NONE', #9192, #396, #10413, .T. ) ;
#13569 = TOROIDAL_SURFACE ( 'NONE', #4998, 0.2999999999999999889, 0.2500000000000000000 ) ;
#13570 = CARTESIAN_POINT ( 'NONE',  ( -1.138568046961029978, -4.362235753495300905, 6.408380708468528475 ) ) ;
#13571 = AXIS2_PLACEMENT_3D ( 'NONE', #17061, #7264, #1707 ) ;
#13572 = DIRECTION ( 'NONE',  ( -1.000000000000000000, -1.306144734853129823E-16, 0.000000000000000000 ) ) ;
#13573 = CARTESIAN_POINT ( 'NONE',  ( 4.225031457058369810E-16, 2.299999999999999822, 7.700000000000000178 ) ) ;
#13574 = CARTESIAN_POINT ( 'NONE',  ( 1.272929729338649674, -0.9155690868286361361, 6.310761232086846917 ) ) ;
#13575 = VERTEX_POINT ( 'NONE', #1556 ) ;
#13576 = LINE ( 'NONE', #9401, #5509 ) ;
#13577 = DIRECTION ( 'NONE',  ( 1.000000000000000000, -8.673617379884035472E-15, 0.000000000000000000 ) ) ;
#13578 = CARTESIAN_POINT ( 'NONE',  ( 1.652654650382400003, -0.7952867690272209522, 3.029252778805620050 ) ) ;
#13579 = CARTESIAN_POINT ( 'NONE',  ( -1.720450724489941852, -2.825208726468270370, 6.720683794561613134 ) ) ;
#13580 = ORIENTED_EDGE ( 'NONE', *, *, #13897, .F. ) ;
#13581 = CARTESIAN_POINT ( 'NONE',  ( -2.500000000000000000, 4.700000000000000178, 1.600000000000000089 ) ) ;
#13582 = DIRECTION ( 'NONE',  ( 0.7071067811865470176, -0.7071067811865480168, 0.000000000000000000 ) ) ;
#13583 = DIRECTION ( 'NONE',  ( -7.401486830834380223E-16, -1.769136588914775099E-30, 1.000000000000000000 ) ) ;
#13584 = CARTESIAN_POINT ( 'NONE',  ( 1.994315313497110997, -5.086440677966105994, 5.187224322759965922 ) ) ;
#13585 = ORIENTED_EDGE ( 'NONE', *, *, #12212, .T. ) ;
#13586 = ORIENTED_EDGE ( 'NONE', *, *, #2746, .F. ) ;
#13587 = CARTESIAN_POINT ( 'NONE',  ( 1.850000000000000089, -5.599999999999999645, 6.899999999999999467 ) ) ;
#13588 = DIRECTION ( 'NONE',  ( 0.000000000000000000, -2.118639217574429265E-16, -1.000000000000000000 ) ) ;
#13589 = CIRCLE ( 'NONE', #2355, 0.2500000000000002220 ) ;
#13590 = DIRECTION ( 'NONE',  ( -1.000000000000000000, 1.224646799147341128E-16, 0.000000000000000000 ) ) ;
#13591 = VERTEX_POINT ( 'NONE', #6163 ) ;
#13592 = CARTESIAN_POINT ( 'NONE',  ( 0.7093417302541469294, -5.435381355932199732, 6.943956659919690466 ) ) ;
#13593 = CARTESIAN_POINT ( 'NONE',  ( 2.603140590302639890, -3.873181699441240244, 5.216500493824248963 ) ) ;
#13594 = CARTESIAN_POINT ( 'NONE',  ( -2.616666666666669805, -4.318079751576579732E-16, 4.000000000000000000 ) ) ;
#13595 = ADVANCED_FACE ( 'NONE', ( #11820 ), #1920, .T. ) ;
#13596 = DIRECTION ( 'NONE',  ( 1.000000000000000000, 0.000000000000000000, 0.000000000000000000 ) ) ;
#13597 = CARTESIAN_POINT ( 'NONE',  ( -3.673940397442036695E-17, 6.700000000000000178, 6.299999999999999822 ) ) ;
#13598 = CARTESIAN_POINT ( 'NONE',  ( -0.2818998297622349880, -4.245794312053860153, 7.036509827384409554 ) ) ;
#13599 = CARTESIAN_POINT ( 'NONE',  ( -0.03000000000000000236, 11.40000000000000036, -2.869354249208270301E-17 ) ) ;
#13600 = CARTESIAN_POINT ( 'NONE',  ( 0.4000000000000000222, 2.399999999999999911, 5.100000000000000533 ) ) ;
#13602 = ORIENTED_EDGE ( 'NONE', *, *, #12778, .T. ) ;
#13601 = CARTESIAN_POINT ( 'NONE',  ( 0.3832714063289482387, -2.914521003261450360, 7.326064873930673294 ) ) ;
#13603 = VECTOR ( 'NONE', #9235, 1000.000000000000000 ) ;
#13604 = DIRECTION ( 'NONE',  ( -1.000000000000000000, -2.220446049250309876E-16, 7.930164461608259947E-17 ) ) ;
#13605 = CARTESIAN_POINT ( 'NONE',  ( -5.045174592681759329E-16, -1.399999999999999911, 5.100000000000000533 ) ) ;
#13606 = CARTESIAN_POINT ( 'NONE',  ( -2.345213174852959881, -1.796683165423619943, 4.503223853122380049 ) ) ;
#13607 = CARTESIAN_POINT ( 'NONE',  ( -2.043308330018790198, -0.5002118644067800046, 5.867646457774669422 ) ) ;
#13608 = DIRECTION ( 'NONE',  ( -5.734623061080349568E-18, 0.000000000000000000, 1.000000000000000000 ) ) ;
#13609 = CARTESIAN_POINT ( 'NONE',  ( -2.345900685764729765, -5.528813559322030002, 4.512231114381339836 ) ) ;
#13610 = VERTEX_POINT ( 'NONE', #17895 ) ;
#13611 = EDGE_CURVE ( 'NONE', #10381, #17781, #892, .T. ) ;
#13612 = SURFACE_STYLE_FILL_AREA ( #7966 ) ;
#13613 = VERTEX_POINT ( 'NONE', #4852 ) ;
#13614 = PLANE ( 'NONE',  #11751 ) ;
#13615 = LINE ( 'NONE', #8065, #10020 ) ;
#13616 = ORIENTED_EDGE ( 'NONE', *, *, #8796, .F. ) ;
#13617 = EDGE_CURVE ( 'NONE', #3744, #1832, #788, .T. ) ;
#13618 = AXIS2_PLACEMENT_3D ( 'NONE', #7390, #7473, #13200 ) ;
#13619 = CARTESIAN_POINT ( 'NONE',  ( 1.728413393879709936, -4.311818300558750039, 6.297289212178290185 ) ) ;
#13620 = ADVANCED_FACE ( 'NONE', ( #16157 ), #3742, .T. ) ;
#13621 = DIRECTION ( 'NONE',  ( -1.000000000000000000, 0.000000000000000000, -1.776356839400249824E-16 ) ) ;
#13622 = CARTESIAN_POINT ( 'NONE',  ( 2.143090896833110381, -5.395338983050850246, 5.672454929438339732 ) ) ;
#13623 = DIRECTION ( 'NONE',  ( -2.220446049250309876E-16, -1.000000000000000000, 0.000000000000000000 ) ) ;
#13624 = CARTESIAN_POINT ( 'NONE',  ( 2.245209214543399945, -2.635061543801989981, 5.405536158119010004 ) ) ;
#13625 = CARTESIAN_POINT ( 'NONE',  ( -0.4446501070882828421, -4.952022267818758650, 2.379695998155090031 ) ) ;
#13626 = CARTESIAN_POINT ( 'NONE',  ( 1.102492180652039577, -2.309025507765959606, 2.968118700883580541 ) ) ;
#13627 = DIRECTION ( 'NONE',  ( -4.898587196589410857E-16, -1.000000000000000000, -4.276423536147510117E-47 ) ) ;
#13628 = VECTOR ( 'NONE', #9410, 1000.000000000000000 ) ;
#13629 = CARTESIAN_POINT ( 'NONE',  ( -1.377628188826471423, -0.5741044150835525883, 2.411088859383701433 ) ) ;
#13630 = ORIENTED_EDGE ( 'NONE', *, *, #13617, .F. ) ;
#13631 = CARTESIAN_POINT ( 'NONE',  ( 1.555847953988059862, -5.162332993428189631, 3.144152046011940094 ) ) ;
#13632 = CARTESIAN_POINT ( 'NONE',  ( 0.1749999999999999889, 8.200000000000001066, 0.4000000000000000222 ) ) ;
#13633 = FILL_AREA_STYLE_COLOUR ( '', #73 ) ;
#13634 = EDGE_LOOP ( 'NONE', ( #319, #11195, #15509, #573 ) ) ;
#13635 = ORIENTED_EDGE ( 'NONE', *, *, #13611, .F. ) ;
#13636 = UNCERTAINTY_MEASURE_WITH_UNIT (LENGTH_MEASURE( 1.000000000000000082E-05 ), #2591, 'distance_accuracy_value', 'NONE');
#13637 = ORIENTED_EDGE ( 'NONE', *, *, #9873, .T. ) ;
#13638 = CARTESIAN_POINT ( 'NONE',  ( -2.053221424930789407, -4.734848366107910600, 3.549770689668290125 ) ) ;
#13639 = CARTESIAN_POINT ( 'NONE',  ( -2.318251751302029984, -5.233262711864409056, 4.294764266798999586 ) ) ;
#13640 = CARTESIAN_POINT ( 'NONE',  ( -2.500000000000000000, 7.299999999999999822, 0.5999999999999999778 ) ) ;
#13641 = VECTOR ( 'NONE', #2856, 1000.000000000000000 ) ;
#13642 = DIRECTION ( 'NONE',  ( 1.110223024625159992E-16, 0.000000000000000000, -1.000000000000000000 ) ) ;
#13643 = CARTESIAN_POINT ( 'NONE',  ( -1.899999999999999911, 11.40000000000000036, 1.600000000000000089 ) ) ;
#13644 = CARTESIAN_POINT ( 'NONE',  ( 0.4735094604799090501, -1.032010528270079996, 7.005327412390689901 ) ) ;
#13645 = CARTESIAN_POINT ( 'NONE',  ( -0.9000000000000000222, -10.00000000000000000, 6.100000000000000533 ) ) ;
#13646 = CARTESIAN_POINT ( 'NONE',  ( -0.5902886515192680150, -1.447358841099289917, 6.978224088050050788 ) ) ;
#13647 = CARTESIAN_POINT ( 'NONE',  ( -2.630358833876468960, -0.2313559322033900412, 4.347767980622416317 ) ) ;
#13648 = ORIENTED_EDGE ( 'NONE', *, *, #8312, .F. ) ;
#13649 = CARTESIAN_POINT ( 'NONE',  ( 2.116444151961470066, -0.3533898305084750002, 3.670839500609349937 ) ) ;
#13650 = VERTEX_POINT ( 'NONE', #7734 ) ;
#13651 = DIRECTION ( 'NONE',  ( -9.251858538542969116E-17, 0.000000000000000000, -1.000000000000000000 ) ) ;
#13652 = CARTESIAN_POINT ( 'NONE',  ( -2.262450597846769718, -1.404623140882690135, 5.348122657979730299 ) ) ;
#13653 = ADVANCED_FACE ( 'NONE', ( #13378, #693, #6330 ), #11994, .F. ) ;
#13654 = CARTESIAN_POINT ( 'NONE',  ( -1.851073041990159984, -5.493220338983049622, 6.153284478378270528 ) ) ;
#13655 = CARTESIAN_POINT ( 'NONE',  ( -0.6919952253609726878, -1.148451969711520082, 7.262080463428013388 ) ) ;
#13656 = VERTEX_POINT ( 'NONE', #11606 ) ;
#13657 = DIRECTION ( 'NONE',  ( 9.796085511398438540E-17, -1.000000000000000000, -6.530723674265629391E-17 ) ) ;
#13658 = CARTESIAN_POINT ( 'NONE',  ( 2.316639661709690046, -3.780028546288089597, 4.285359956977719875 ) ) ;
#13659 = PLANE ( 'NONE',  #7298 ) ;
#13660 = FACE_OUTER_BOUND ( 'NONE', #15226, .T. ) ;
#13661 = CARTESIAN_POINT ( 'NONE',  ( -1.872456193198849705, -4.501965483225034426, 5.541908336566010007 ) ) ;
#13662 = FACE_OUTER_BOUND ( 'NONE', #12903, .T. ) ;
#13663 = CARTESIAN_POINT ( 'NONE',  ( 0.03000000000000110217, 11.40000000000000036, 1.600000000000000089 ) ) ;
#13664 = CARTESIAN_POINT ( 'NONE',  ( -0.5805547688319036004, -3.360839357098899693, 2.730772231808969774 ) ) ;
#13665 = VERTEX_POINT ( 'NONE', #17326 ) ;
#13666 = CARTESIAN_POINT ( 'NONE',  ( -0.02999999999999520064, 12.00000000000000000, 7.649999999999999467 ) ) ;
#13667 = DIRECTION ( 'NONE',  ( -1.000000000000000000, 0.000000000000000000, 0.000000000000000000 ) ) ;
#13668 = EDGE_CURVE ( 'NONE', #2762, #2627, #7366, .T. ) ;
#13669 = CARTESIAN_POINT ( 'NONE',  ( 1.545075033357670158, -0.4774152569121719591, 2.920238509828300355 ) ) ;
#13670 = CARTESIAN_POINT ( 'NONE',  ( 1.236224677598260158, -1.986830348089900777, 2.351625617688071657 ) ) ;
#13671 = EDGE_LOOP ( 'NONE', ( #5344, #4984, #5789, #11932 ) ) ;
#13672 = DIRECTION ( 'NONE',  ( -4.440892098500630106E-16, 0.000000000000000000, 1.000000000000000000 ) ) ;
#13673 = CARTESIAN_POINT ( 'NONE',  ( -0.7500000000000000000, 6.450000000000000178, 3.200000000000000178 ) ) ;
#13674 = CARTESIAN_POINT ( 'NONE',  ( -2.012177589105470066, -5.215466101694915757, 5.107213040360599088 ) ) ;
#13675 = ORIENTED_EDGE ( 'NONE', *, *, #2414, .F. ) ;
#13676 = EDGE_CURVE ( 'NONE', #17390, #11415, #4657, .T. ) ;
#13677 = VECTOR ( 'NONE', #5988, 1000.000000000000000 ) ;
#13678 = ORIENTED_EDGE ( 'NONE', *, *, #10868, .F. ) ;
#13679 = FACE_OUTER_BOUND ( 'NONE', #12110, .T. ) ;
#13680 = ADVANCED_FACE ( 'NONE', ( #10131 ), #1882, .T. ) ;
#13681 = DIRECTION ( 'NONE',  ( -0.000000000000000000, 1.000000000000000000, 0.000000000000000000 ) ) ;
#13682 = CYLINDRICAL_SURFACE ( 'NONE', #2281, 0.1000000000000002554 ) ;
#13683 = EDGE_CURVE ( 'NONE', #17967, #17304, #8740, .T. ) ;
#13684 = EDGE_LOOP ( 'NONE', ( #5348, #17474, #4705, #2733 ) ) ;
#13685 = CARTESIAN_POINT ( 'NONE',  ( 2.350067830300900162, -5.377542372881360500, 4.825253242917690422 ) ) ;
#13686 = CARTESIAN_POINT ( 'NONE',  ( 1.670747221194369914, -0.4963798976394459550, 3.047345349617600174 ) ) ;
#13687 = CARTESIAN_POINT ( 'NONE',  ( 0.009452039534070141164, -0.3001931771041043140, 2.350000000173209092 ) ) ;
#13688 = CARTESIAN_POINT ( 'NONE',  ( -2.295344368707641358, -3.473439922180372452, 3.367893426919611688 ) ) ;
#13689 = PLANE ( 'NONE',  #14695 ) ;
#13690 = CARTESIAN_POINT ( 'NONE',  ( 1.854177340199709922, -3.989623140882689434, 6.149404042554680316 ) ) ;
#13691 = DIRECTION ( 'NONE',  ( 4.476422471267168520E-17, 0.6823182503600082605, 0.7310552682428719251 ) ) ;
#13692 = DIRECTION ( 'NONE',  ( -5.551115123125779621E-17, 0.000000000000000000, -1.000000000000000000 ) ) ;
#13693 = CIRCLE ( 'NONE', #7191, 0.01000000000000002623 ) ;
#13695 = ORIENTED_EDGE ( 'NONE', *, *, #11591, .F. ) ;
#13694 = CARTESIAN_POINT ( 'NONE',  ( 2.212163452524050111, -2.704926408666860738, 6.166099093621837390 ) ) ;
#13696 = DIRECTION ( 'NONE',  ( 0.000000000000000000, 0.000000000000000000, 1.000000000000000000 ) ) ;
#13697 = CARTESIAN_POINT ( 'NONE',  ( 2.116444151961470066, -0.3533898305084750002, 3.670839500609349937 ) ) ;
#13698 = CARTESIAN_POINT ( 'NONE',  ( -0.8429265834919730249, -2.076142624883080323, 2.502678798553459760 ) ) ;
#13699 = CARTESIAN_POINT ( 'NONE',  ( -1.477796163681079911, -0.4824152542372879826, 6.531563725478150673 ) ) ;
#13700 = FACE_OUTER_BOUND ( 'NONE', #4077, .T. ) ;
#13701 = CARTESIAN_POINT ( 'NONE',  ( 2.304156201936080617, -5.399788135593215799, 6.016707707703351282 ) ) ;
#13702 = ORIENTED_EDGE ( 'NONE', *, *, #7219, .F. ) ;
#13703 = ADVANCED_FACE ( 'NONE', ( #8923 ), #10050, .F. ) ;
#13704 =( NAMED_UNIT ( * ) SI_UNIT ( $, .STERADIAN. ) SOLID_ANGLE_UNIT ( ) );
#13705 = CARTESIAN_POINT ( 'NONE',  ( 0.9150601050661637537, -5.130932203389829027, 6.868218666554229301 ) ) ;
#13706 = CARTESIAN_POINT ( 'NONE',  ( -1.800000000000000044, 11.29999999999999893, 1.600000000000000089 ) ) ;
#13707 = DIRECTION ( 'NONE',  ( 3.652293603810800245E-15, 1.332267629550185876E-15, -1.000000000000000000 ) ) ;
#13708 = ORIENTED_EDGE ( 'NONE', *, *, #11874, .F. ) ;
#13709 = CARTESIAN_POINT ( 'NONE',  ( 1.021156010535390068, -3.846052534792979927, 2.579625955254269964 ) ) ;
#13710 = CARTESIAN_POINT ( 'NONE',  ( 1.791574935211219799, -5.408686440677969998, 6.226029630577610163 ) ) ;
#13711 = DIRECTION ( 'NONE',  ( -1.000000000000000000, 0.000000000000000000, 6.123233995736769734E-17 ) ) ;
#13712 = CARTESIAN_POINT ( 'NONE',  ( -1.816660071039029933, -3.170692174432619748, 6.196159040268240936 ) ) ;
#13713 = DIRECTION ( 'NONE',  ( 0.7071067811865461294, 1.385375698838618738E-16, -0.7071067811865490160 ) ) ;
#13714 = CARTESIAN_POINT ( 'NONE',  ( 0.01333550863827670518, -2.169295778036230526, 2.647020699851690306 ) ) ;
#13715 = CARTESIAN_POINT ( 'NONE',  ( -2.500000000000000000, 2.000000000000000000, 1.600000000000000089 ) ) ;
#13716 = CARTESIAN_POINT ( 'NONE',  ( -0.5058614788087384406, -0.2909039927201511055, 2.084176093893880921 ) ) ;
#13717 = ORIENTED_EDGE ( 'NONE', *, *, #12855, .F. ) ;
#13718 = ADVANCED_FACE ( 'NONE', ( #14569 ), #238, .F. ) ;
#13719 = DIRECTION ( 'NONE',  ( -1.216682766712499758E-16, 6.416248801027068947E-32, -1.000000000000000000 ) ) ;
#13720 = CARTESIAN_POINT ( 'NONE',  ( -1.951437470830620136, -5.057043525783970317, 3.384463041838880137 ) ) ;
#13721 = ORIENTED_EDGE ( 'NONE', *, *, #5902, .T. ) ;
#13722 = ORIENTED_EDGE ( 'NONE', *, *, #12076, .F. ) ;
#13723 = ORIENTED_EDGE ( 'NONE', *, *, #2695, .T. ) ;
#13724 = DIRECTION ( 'NONE',  ( -6.938893903907229610E-17, 0.000000000000000000, -1.000000000000000000 ) ) ;
#13725 = CARTESIAN_POINT ( 'NONE',  ( 2.143090896833110381, -5.095338983050850423, 5.672454929438339732 ) ) ;
#13726 = CARTESIAN_POINT ( 'NONE',  ( -0.1749999999999999889, 9.299999999999998934, 1.600000000000000089 ) ) ;
#13727 = LINE ( 'NONE', #1137, #4033 ) ;
#13728 = APPLICATION_CONTEXT ( 'automotive_design' ) ;
#13729 = CARTESIAN_POINT ( 'NONE',  ( 1.670747221194369914, -0.4963798976394459550, 3.047345349617600174 ) ) ;
#13730 = DIRECTION ( 'NONE',  ( 1.000000000000000000, 0.000000000000000000, 0.000000000000000000 ) ) ;
#13731 = CARTESIAN_POINT ( 'NONE',  ( 1.644832646965660006, -1.191187669928119863, 6.383232381746459794 ) ) ;
#13732 = CARTESIAN_POINT ( 'NONE',  ( -1.666450993087168930, -0.1824152542372889096, 6.765380371283871597 ) ) ;
#13733 = CARTESIAN_POINT ( 'NONE',  ( -2.350067830300900162, -0.5224576271186440746, 4.825253242917699303 ) ) ;
#13734 = VECTOR ( 'NONE', #1927, 1000.000000000000000 ) ;
#13735 = EDGE_LOOP ( 'NONE', ( #9841, #5664, #977, #16077 ) ) ;
#13736 = CARTESIAN_POINT ( 'NONE',  ( 0.2189795514005130062, -0.004449152542373159894, 2.356806637999009801 ) ) ;
#13737 = DIRECTION ( 'NONE',  ( 1.168655815394900078E-16, -1.000000000000000000, -1.110223024625159992E-16 ) ) ;
#13738 = CARTESIAN_POINT ( 'NONE',  ( 2.161802606005189809, -0.5895330507925999886, 3.769755311421790989 ) ) ;
#13739 = CARTESIAN_POINT ( 'NONE',  ( -2.203023580853999963, -5.542161016949149754, 3.872235369154300333 ) ) ;
#13740 = CARTESIAN_POINT ( 'NONE',  ( -2.248786803694121428, -1.334758276017820267, 6.109280527266697014 ) ) ;
#13741 = ORIENTED_EDGE ( 'NONE', *, *, #1665, .T. ) ;
#13742 = DIRECTION ( 'NONE',  ( -1.000000000000000000, 0.000000000000000000, 0.000000000000000000 ) ) ;
#13743 = CARTESIAN_POINT ( 'NONE',  ( -2.329383452786330189, -4.571830348089889640, 5.035735636132879556 ) ) ;
#13744 = CARTESIAN_POINT ( 'NONE',  ( -0.1749999999999999889, 9.199999999999999289, 0.4000000000000000222 ) ) ;
#13745 = CARTESIAN_POINT ( 'NONE',  ( -0.2335786437626909962, 6.450000000000000178, 2.241421356237310203 ) ) ;
#13746 = CARTESIAN_POINT ( 'NONE',  ( -1.876226141297921091, -4.711560077819614278, 3.866526959224360294 ) ) ;
#13747 = CARTESIAN_POINT ( 'NONE',  ( 2.500000000000000000, 9.199999999999999289, 1.600000000000000089 ) ) ;
#13748 = EDGE_LOOP ( 'NONE', ( #9372, #10032, #12589, #7099 ) ) ;
#13749 = DIRECTION ( 'NONE',  ( -1.000000000000000000, 0.000000000000000000, 0.000000000000000000 ) ) ;
#13750 = DIRECTION ( 'NONE',  ( 1.110223024625159992E-16, 0.000000000000000000, 1.000000000000000000 ) ) ;
#13751 = CARTESIAN_POINT ( 'NONE',  ( -1.795861365445549973, -0.2491525423728821742, 3.705232155007899930 ) ) ;
#13752 = CARTESIAN_POINT ( 'NONE',  ( 2.649291707874080970, -2.243001519261071053, 4.543900225523779035 ) ) ;
#13753 = DIRECTION ( 'NONE',  ( 0.000000000000000000, 0.000000000000000000, 1.000000000000000000 ) ) ;
#13754 = PLANE ( 'NONE',  #15983 ) ;
#13755 = CARTESIAN_POINT ( 'NONE',  ( 1.562863241354470523, -5.408686440677975327, 6.031217337312382298 ) ) ;
#13756 = ORIENTED_EDGE ( 'NONE', *, *, #8581, .F. ) ;
#13757 = CARTESIAN_POINT ( 'NONE',  ( 0.1749999999999999889, 9.500000000000000000, 1.600000000000000089 ) ) ;
#13758 = CARTESIAN_POINT ( 'NONE',  ( 1.943632316591230147, -5.346398305084740343, 3.373048379518159834 ) ) ;
#13759 = LINE ( 'NONE', #2393, #13515 ) ;
#13760 = ORIENTED_EDGE ( 'NONE', *, *, #1836, .F. ) ;
#13761 = CARTESIAN_POINT ( 'NONE',  ( -3.503171016405825766E-15, -5.600000000000000533, 2.649999999999998579 ) ) ;
#13762 = CARTESIAN_POINT ( 'NONE',  ( 2.358786130710011086, -3.943046564306109669, 5.916240799583690979 ) ) ;
#13763 = CARTESIAN_POINT ( 'NONE',  ( 1.152986057739970205, -3.846052534792983923, 2.309657588616410351 ) ) ;
#13764 = CARTESIAN_POINT ( 'NONE',  ( 2.500000000000000000, 2.799999999999999822, 0.5999999999999999778 ) ) ;
#13765 = CARTESIAN_POINT ( 'NONE',  ( 2.051973656473811136, -0.6826862039457533005, 4.634380218157459375 ) ) ;
#13766 = EDGE_CURVE ( 'NONE', #138, #4659, #7530, .T. ) ;
#13767 = CARTESIAN_POINT ( 'NONE',  ( -0.1749999999999999889, 7.900000000000000355, 0.5999999999999999778 ) ) ;
#13768 = FACE_OUTER_BOUND ( 'NONE', #15274, .T. ) ;
#13769 = VERTEX_POINT ( 'NONE', #13174 ) ;
#13770 = EDGE_CURVE ( 'NONE', #4320, #6296, #491, .T. ) ;
#13771 = EDGE_CURVE ( 'NONE', #14262, #2153, #3280, .T. ) ;
#13772 = DIRECTION ( 'NONE',  ( 2.220446049250309876E-16, 5.551115123125779621E-17, -1.000000000000000000 ) ) ;
#13773 = CARTESIAN_POINT ( 'NONE',  ( -1.477796163681079911, -0.4824152542372879826, 6.531563725478150673 ) ) ;
#13774 = CARTESIAN_POINT ( 'NONE',  ( 2.276802572547980130, -2.495331814072260013, 4.104251954998760610 ) ) ;
#13775 = LINE ( 'NONE', #6745, #2156 ) ;
#13776 = CARTESIAN_POINT ( 'NONE',  ( -0.1698804968610999888, -0.2965485159365569556, 2.349238660949160007 ) ) ;
#13777 = CARTESIAN_POINT ( 'NONE',  ( 2.586172839791708533, -5.064194915254235596, 4.104546363490936045 ) ) ;
#13778 = ORIENTED_EDGE ( 'NONE', *, *, #16166, .T. ) ;
#13779 = PRODUCT_DEFINITION_SHAPE ( 'NONE', 'NONE',  #18295 ) ;
#13780 = CARTESIAN_POINT ( 'NONE',  ( -3.399999999999999911, -9.500000000000000000, 3.799999999999999822 ) ) ;
#13781 = CYLINDRICAL_SURFACE ( 'NONE', #5504, 0.3499999999999996447 ) ;
#13782 = DIRECTION ( 'NONE',  ( -2.261565420532729920E-16, -1.000000000000000000, 0.000000000000000000 ) ) ;
#13783 = VECTOR ( 'NONE', #12266, 1000.000000000000000 ) ;
#13784 = ORIENTED_EDGE ( 'NONE', *, *, #3073, .F. ) ;
#13785 = CARTESIAN_POINT ( 'NONE',  ( -2.137408332595969629, -3.450151633892079683, 3.714996798363980002 ) ) ;
#13786 = EDGE_CURVE ( 'NONE', #6595, #14665, #12927, .T. ) ;
#13787 = SURFACE_SIDE_STYLE ('',( #13969 ) ) ;
#13788 = CARTESIAN_POINT ( 'NONE',  ( -1.399999999999999911, 0.5999999999999999778, 3.299999999999999822 ) ) ;
#13789 = DIRECTION ( 'NONE',  ( 0.000000000000000000, 0.000000000000000000, -1.000000000000000000 ) ) ;
#13790 = EDGE_CURVE ( 'NONE', #11075, #17860, #6140, .T. ) ;
#13791 = DIRECTION ( 'NONE',  ( 0.000000000000000000, -1.000000000000000000, -6.049014748177290126E-16 ) ) ;
#13792 = CARTESIAN_POINT ( 'NONE',  ( -2.334032080503389839, -3.310421904162350160, 5.001728246382240783 ) ) ;
#13793 = EDGE_CURVE ( 'NONE', #16687, #2627, #8198, .T. ) ;
#13794 = CARTESIAN_POINT ( 'NONE',  ( -2.065623031241579977, -5.033755237495680213, 3.572193642975310279 ) ) ;
#13795 = AXIS2_PLACEMENT_3D ( 'NONE', #2264, #972, #8019 ) ;
#13796 = CARTESIAN_POINT ( 'NONE',  ( 0.5805547688318586363, -2.239160642901089293, 2.730772231808960449 ) ) ;
#13797 = AXIS2_PLACEMENT_3D ( 'NONE', #17984, #9664, #5330 ) ;
#13798 = DIRECTION ( 'NONE',  ( 1.000000000000000000, -1.899065700016719806E-16, 0.000000000000000000 ) ) ;
#13799 = CARTESIAN_POINT ( 'NONE',  ( -0.9193620247240871235, -0.2831443699174389095, 2.206709149717571261 ) ) ;
#13800 = ORIENTED_EDGE ( 'NONE', *, *, #16513, .T. ) ;
#13801 = CARTESIAN_POINT ( 'NONE',  ( 0.1749999999999999889, 4.299999999999999822, 1.600000000000000089 ) ) ;
#13802 = ORIENTED_EDGE ( 'NONE', *, *, #6495, .T. ) ;
#13803 = VERTEX_POINT ( 'NONE', #15706 ) ;
#13804 = AXIS2_PLACEMENT_3D ( 'NONE', #1457, #16992, #4305 ) ;
#13805 = UNCERTAINTY_MEASURE_WITH_UNIT (LENGTH_MEASURE( 1.000000000000000082E-05 ), #6078, 'distance_accuracy_value', 'NONE');
#13806 = VERTEX_POINT ( 'NONE', #11697 ) ;
#13807 = DIRECTION ( 'NONE',  ( -4.440892098500620245E-16, 3.700743415417219694E-16, -1.000000000000000000 ) ) ;
#13808 = CARTESIAN_POINT ( 'NONE',  ( 2.034805890357269220, -5.068644067796615360, 4.427518626519221456 ) ) ;
#13809 = VECTOR ( 'NONE', #17189, 1000.000000000000000 ) ;
#13810 = DIRECTION ( 'NONE',  ( 1.000000000000000000, 0.000000000000000000, 0.000000000000000000 ) ) ;
#13811 = VECTOR ( 'NONE', #17152, 1000.000000000000000 ) ;
#13812 = CARTESIAN_POINT ( 'NONE',  ( 1.890000000000029878, 4.100000000000000533, 3.000000000000000000 ) ) ;
#13813 = DIRECTION ( 'NONE',  ( 1.000000000000000000, 0.000000000000000000, 1.168655815394900078E-16 ) ) ;
#13814 = CARTESIAN_POINT ( 'NONE',  ( -2.306572132003601450, -4.478677194936736328, 6.012569500204175910 ) ) ;
#13815 = EDGE_CURVE ( 'NONE', #17593, #14776, #2890, .T. ) ;
#13816 = DIRECTION ( 'NONE',  ( -1.000000000000000000, 0.000000000000000000, 0.000000000000000000 ) ) ;
#13817 = CARTESIAN_POINT ( 'NONE',  ( 1.303621121494459967, -1.237764246504700072, 6.659417683669679455 ) ) ;
#13818 = AXIS2_PLACEMENT_3D ( 'NONE', #17906, #13590, #9682 ) ;
#13819 = CARTESIAN_POINT ( 'NONE',  ( 1.438959988998139914E-16, -2.775557561562889872E-16, 2.350000000000000089 ) ) ;
#13820 = ORIENTED_EDGE ( 'NONE', *, *, #10737, .T. ) ;
#13821 = CARTESIAN_POINT ( 'NONE',  ( -1.925796468768790071, -0.4957627118644070130, 6.052706598917719560 ) ) ;
#13822 = CARTESIAN_POINT ( 'NONE',  ( -2.051331987628511211, -0.5269067796610176213, 4.618035453557344461 ) ) ;
#13823 = EDGE_CURVE ( 'NONE', #15295, #11463, #11524, .T. ) ;
#13824 = ORIENTED_EDGE ( 'NONE', *, *, #5352, .T. ) ;
#13825 = VECTOR ( 'NONE', #2266, 1000.000000000000000 ) ;
#13826 = CARTESIAN_POINT ( 'NONE',  ( -0.3171869470818471370, -0.1557203389830511819, 7.334814496515233095 ) ) ;
#13827 = VECTOR ( 'NONE', #14136, 1000.000000000000000 ) ;
#13828 = ORIENTED_EDGE ( 'NONE', *, *, #13021, .T. ) ;
#13829 = DIRECTION ( 'NONE',  ( -2.220446049250309876E-16, -1.000000000000000000, 1.850371707708589879E-16 ) ) ;
#13830 = EDGE_CURVE ( 'NONE', #16687, #6171, #15308, .T. ) ;
#13831 = CARTESIAN_POINT ( 'NONE',  ( -0.5570002967655938164, -2.708767285026831395, 6.986590552960220357 ) ) ;
#13832 = CARTESIAN_POINT ( 'NONE',  ( -2.353194804772640314, -5.524364406779660008, 4.731327187377240229 ) ) ;
#13833 = CIRCLE ( 'NONE', #3179, 0.7000000000000000666 ) ;
#13834 = CARTESIAN_POINT ( 'NONE',  ( -2.437122747866789840, -5.010466949207390108, 3.649501829874993941 ) ) ;
#13835 = ORIENTED_EDGE ( 'NONE', *, *, #6467, .F. ) ;
#13836 = DIRECTION ( 'NONE',  ( 1.000000000000000000, 0.000000000000000000, 0.000000000000000000 ) ) ;
#13837 = CARTESIAN_POINT ( 'NONE',  ( 2.049150047780149642, -0.7059744922340407403, 4.826039376028505856 ) ) ;
#13838 = CARTESIAN_POINT ( 'NONE',  ( -2.649108131072720695, -4.894025507765944916, 4.859184807329705258 ) ) ;
#13839 = EDGE_CURVE ( 'NONE', #13271, #8528, #4083, .T. ) ;
#13840 = AXIS2_PLACEMENT_3D ( 'NONE', #10508, #704, #17620 ) ;
#13841 = DIRECTION ( 'NONE',  ( 0.000000000000000000, 0.000000000000000000, -1.000000000000000000 ) ) ;
#13842 = CARTESIAN_POINT ( 'NONE',  ( -0.3257255101953093757, -1.424070552811000701, 6.727018681373241549 ) ) ;
#13843 = CARTESIAN_POINT ( 'NONE',  ( -1.889999999999999902, 3.500000000000000000, 0.6099999999999999867 ) ) ;
#13844 = VERTEX_POINT ( 'NONE', #15407 ) ;
#13845 = PLANE ( 'NONE',  #15179 ) ;
#13846 = FACE_OUTER_BOUND ( 'NONE', #12559, .T. ) ;
#13847 = VECTOR ( 'NONE', #2028, 1000.000000000000000 ) ;
#13848 = CARTESIAN_POINT ( 'NONE',  ( 1.980638384804650931, -0.3622881355932213721, 4.159858630563753934 ) ) ;
#13849 = VECTOR ( 'NONE', #11462, 1000.000000000000000 ) ;
#13850 = EDGE_CURVE ( 'NONE', #11463, #4854, #9918, .T. ) ;
#13851 = CARTESIAN_POINT ( 'NONE',  ( 1.011820239713300484, -1.963542059801608897, 2.246566997958089118 ) ) ;
#13852 = CARTESIAN_POINT ( 'NONE',  ( -1.676695548152530968, -4.829629811528105776, 2.630596693608521885 ) ) ;
#13853 = CARTESIAN_POINT ( 'NONE',  ( -1.392553072310521278, -5.264406779661021218, 3.191531554476531252 ) ) ;
#13854 = ORIENTED_EDGE ( 'NONE', *, *, #2963, .F. ) ;
#13855 = AXIS2_PLACEMENT_3D ( 'NONE', #9170, #17570, #7603 ) ;
#13856 = CARTESIAN_POINT ( 'NONE',  ( 1.399999999999999911, -5.500000000000000000, 5.100000000000000533 ) ) ;
#13857 = CARTESIAN_POINT ( 'NONE',  ( 1.850000000000000089, 11.25000000000000000, 7.649999999999999467 ) ) ;
#13858 = DIRECTION ( 'NONE',  ( 0.000000000000000000, 0.000000000000000000, 1.000000000000000000 ) ) ;
#13859 = ORIENTED_EDGE ( 'NONE', *, *, #15047, .T. ) ;
#13860 = CARTESIAN_POINT ( 'NONE',  ( -0.5889081234606770021, -5.462076271186440124, 6.978529000034869867 ) ) ;
#13861 = VECTOR ( 'NONE', #15366, 1000.000000000000000 ) ;
#13862 = VECTOR ( 'NONE', #14704, 1000.000000000000000 ) ;
#13863 = CARTESIAN_POINT ( 'NONE',  ( -2.651429253058529945, -4.618406924666464519, 4.585822029124955179 ) ) ;
#13864 = CARTESIAN_POINT ( 'NONE',  ( 2.470260739716200860, -4.032358841099289215, 3.729986819255199926 ) ) ;
#13865 = DIRECTION ( 'NONE',  ( -1.224646799147350002E-16, 1.000000000000000000, 6.123233995736759873E-17 ) ) ;
#13866 = CARTESIAN_POINT ( 'NONE',  ( -1.741179788930630190, -1.334758276017820267, 5.787747574231985936 ) ) ;
#13867 = PLANE ( 'NONE',  #14092 ) ;
#13868 = CARTESIAN_POINT ( 'NONE',  ( -0.6500000000000000222, 6.450000000000000178, 3.200000000000000178 ) ) ;
#13869 = EDGE_LOOP ( 'NONE', ( #15215, #11137, #5230, #3502 ) ) ;
#13870 = EDGE_CURVE ( 'NONE', #7652, #5300, #16768, .T. ) ;
#13871 = DIRECTION ( 'NONE',  ( 0.7045302523384989746, -0.08528919673497019349, -0.7045302523385029714 ) ) ;
#13872 = CARTESIAN_POINT ( 'NONE',  ( 2.653602652190420574, -0.3756355932203404024, 4.735326402787084277 ) ) ;
#13873 = VECTOR ( 'NONE', #10511, 1000.000000000000000 ) ;
#13874 = CARTESIAN_POINT ( 'NONE',  ( 1.866416942370620058, -3.962493976234419790, 3.266391446483460026 ) ) ;
#13875 = CARTESIAN_POINT ( 'NONE',  ( -0.004607033757067210099, -5.223017583943910580, 2.216967106706590140 ) ) ;
#13876 = DIRECTION ( 'NONE',  ( 1.224646799147350002E-16, -1.000000000000000000, -6.123233995736769734E-17 ) ) ;
#13877 = CARTESIAN_POINT ( 'NONE',  ( -2.230812463554230352, -5.497669491525425833, 6.137473736419926773 ) ) ;
#13878 = ORIENTED_EDGE ( 'NONE', *, *, #4833, .F. ) ;
#13879 = ORIENTED_EDGE ( 'NONE', *, *, #13224, .F. ) ;
#13880 = CARTESIAN_POINT ( 'NONE',  ( -2.253200202764409354, -5.211016949152539546, 5.379408587037509903 ) ) ;
#13881 = PLANE ( 'NONE',  #7868 ) ;
#13882 = DIRECTION ( 'NONE',  ( 1.000000000000000000, 0.000000000000000000, 0.000000000000000000 ) ) ;
#13883 = ORIENTED_EDGE ( 'NONE', *, *, #11451, .T. ) ;
#13884 = EDGE_CURVE ( 'NONE', #8433, #9237, #2711, .T. ) ;
#13885 = CARTESIAN_POINT ( 'NONE',  ( -0.6918414964982418924, -3.659746228486680408, 2.450533167346770291 ) ) ;
#13886 = CARTESIAN_POINT ( 'NONE',  ( -0.9000000000000000222, 2.050000000000000266, 3.600000000000000089 ) ) ;
#13887 = CARTESIAN_POINT ( 'NONE',  ( 0.6410058658986126368, -5.311531839079355777, 2.106117395030960626 ) ) ;
#13888 = VECTOR ( 'NONE', #11918, 1000.000000000000000 ) ;
#13889 = DIRECTION ( 'NONE',  ( -1.746418240983389920E-16, 1.000000000000000000, 0.000000000000000000 ) ) ;
#13890 = CARTESIAN_POINT ( 'NONE',  ( -0.5999999999999999778, 10.80000000000000071, 7.599999999999999645 ) ) ;
#13891 = CARTESIAN_POINT ( 'NONE',  ( -2.349464193210359930, -3.356998480738930368, 4.563019372514619754 ) ) ;
#13892 = CARTESIAN_POINT ( 'NONE',  ( -0.1686436619862690112, -4.981295943764798118, 2.349239845786320391 ) ) ;
#13893 = CARTESIAN_POINT ( 'NONE',  ( -1.555285212483289659, -3.520016498756949552, 3.359854578615099285 ) ) ;
#13894 = CARTESIAN_POINT ( 'NONE',  ( 2.500000000000000000, 0.8000000000000000444, -1.769429514865259726E-15 ) ) ;
#13895 = DIRECTION ( 'NONE',  ( -2.220446049250309876E-16, -5.551115123125779621E-17, 1.000000000000000000 ) ) ;
#13896 = ORIENTED_EDGE ( 'NONE', *, *, #2191, .T. ) ;
#13897 = EDGE_CURVE ( 'NONE', #15169, #5684, #16866, .T. ) ;
#13898 = CARTESIAN_POINT ( 'NONE',  ( -2.161802606005209793, -5.010466949207389220, 3.769755311421840283 ) ) ;
#13899 = ORIENTED_EDGE ( 'NONE', *, *, #8639, .T. ) ;
#13900 = VECTOR ( 'NONE', #13225, 1000.000000000000000 ) ;
#13901 = ORIENTED_EDGE ( 'NONE', *, *, #17159, .T. ) ;
#13902 = EDGE_CURVE ( 'NONE', #15551, #6826, #15307, .T. ) ;
#13903 = ADVANCED_FACE ( 'NONE', ( #15577 ), #7067, .F. ) ;
#13904 = EDGE_LOOP ( 'NONE', ( #17856, #6366, #11091, #12751 ) ) ;
#13905 = DIRECTION ( 'NONE',  ( 6.123233995736769734E-17, 8.894960955186829541E-48, 1.000000000000000000 ) ) ;
#13906 = EDGE_CURVE ( 'NONE', #12624, #11239, #17122, .T. ) ;
#13907 = CARTESIAN_POINT ( 'NONE',  ( -2.041338374031088865, -5.219915254237295521, 4.918217215283674726 ) ) ;
#13908 = EDGE_CURVE ( 'NONE', #5745, #796, #2292, .T. ) ;
#13909 = CARTESIAN_POINT ( 'NONE',  ( -1.945845091386011250, -1.660794312053860633, 2.895339208235828909 ) ) ;
#13910 = FACE_OUTER_BOUND ( 'NONE', #9146, .T. ) ;
#13911 = FACE_OUTER_BOUND ( 'NONE', #4458, .T. ) ;
#13912 = DIRECTION ( 'NONE',  ( 1.908195823574489776E-16, -1.000000000000000000, -6.938893903907229610E-17 ) ) ;
#13913 = CARTESIAN_POINT ( 'NONE',  ( -1.670747221194380128, -5.103620102360550526, 3.047345349617600174 ) ) ;
#13914 = DIRECTION ( 'NONE',  ( 1.000000000000000000, 0.000000000000000000, -5.332141831895923026E-16 ) ) ;
#13915 = CIRCLE ( 'NONE', #2385, 0.2500000000000002220 ) ;
#13916 = CARTESIAN_POINT ( 'NONE',  ( -2.340959815966380031, -1.750106588847040179, 4.942183458383479611 ) ) ;
#13917 = CARTESIAN_POINT ( 'NONE',  ( -1.031876288691620625, -0.1690677966101698793, 7.145012538880312292 ) ) ;
#13918 = CARTESIAN_POINT ( 'NONE',  ( 0.5889081234606849957, -0.4379237288135600092, 6.978529000034869867 ) ) ;
#13919 = EDGE_LOOP ( 'NONE', ( #9186, #12221, #9990, #10354 ) ) ;
#13920 = CARTESIAN_POINT ( 'NONE',  ( -1.925796468768790071, -0.1957627118644069963, 6.052706598917719560 ) ) ;
#13921 = CARTESIAN_POINT ( 'NONE',  ( 2.053221424930760097, -0.8651516338920849369, 3.549770689668250157 ) ) ;
#13922 = ORIENTED_EDGE ( 'NONE', *, *, #2634, .T. ) ;
#13923 = LINE ( 'NONE', #1241, #11780 ) ;
#13924 = ADVANCED_FACE ( 'NONE', ( #13911 ), #6955, .T. ) ;
#13925 = CARTESIAN_POINT ( 'NONE',  ( 1.816660071039059465, -2.429307825567370571, 6.196159040268200968 ) ) ;
#13926 = VECTOR ( 'NONE', #9001, 1000.000000000000000 ) ;
#13927 = CARTESIAN_POINT ( 'NONE',  ( 1.666450993087180477, -5.417584745762705545, 6.765380371283858274 ) ) ;
#13928 = VERTEX_POINT ( 'NONE', #1403 ) ;
#13929 = CARTESIAN_POINT ( 'NONE',  ( -1.552749016687749783, -1.563800282540730002, 6.468535037441760061 ) ) ;
#13930 = CARTESIAN_POINT ( 'NONE',  ( -1.652654650382400003, -4.804713230972780025, 3.029252778805629820 ) ) ;
#13931 = VERTEX_POINT ( 'NONE', #13990 ) ;
#13932 = CARTESIAN_POINT ( 'NONE',  ( 6.735557395310435121E-17, 2.600000000000000089, 8.250000000000000000 ) ) ;
#13933 = LINE ( 'NONE', #231, #4202 ) ;
#13934 = CARTESIAN_POINT ( 'NONE',  ( -1.998374131852739266, -4.664983501243040287, 4.229465546630535755 ) ) ;
#13935 = PRODUCT ( 'Solder Terminal Pins', 'Solder Terminal Pins', '', ( #12155 ) ) ;
#13936 = DIRECTION ( 'NONE',  ( 1.000000000000000000, 0.000000000000000000, 0.000000000000000000 ) ) ;
#13937 = EDGE_LOOP ( 'NONE', ( #16673, #2320, #14628, #12512 ) ) ;
#13938 = FACE_OUTER_BOUND ( 'NONE', #15341, .T. ) ;
#13939 = DIRECTION ( 'NONE',  ( -0.000000000000000000, 1.000000000000000000, 0.000000000000000000 ) ) ;
#13940 = CARTESIAN_POINT ( 'NONE',  ( -2.034805890357269220, -0.2313559322033900412, 4.427518626519226785 ) ) ;
#13941 = CARTESIAN_POINT ( 'NONE',  ( 1.597383073937500786, -3.593722239981783861, 2.580688553303249755 ) ) ;
#13942 = ORIENTED_EDGE ( 'NONE', *, *, #15636, .F. ) ;
#13943 = CARTESIAN_POINT ( 'NONE',  ( -0.7252674547190166576, -5.211074464177385401, 2.776474344060209987 ) ) ;
#13944 = CARTESIAN_POINT ( 'NONE',  ( -1.901882987994748975, -5.206567796610170440, 5.472995608211450147 ) ) ;
#13945 = EDGE_LOOP ( 'NONE', ( #13106, #14049, #12051, #3414 ) ) ;
#13946 = EDGE_CURVE ( 'NONE', #17729, #6294, #1308, .T. ) ;
#13947 = CARTESIAN_POINT ( 'NONE',  ( 2.345900685764729765, -0.07118644067796647823, 4.512231114381329178 ) ) ;
#13948 = DIRECTION ( 'NONE',  ( -1.224646799147350002E-16, 8.383884571949770538E-16, -1.000000000000000000 ) ) ;
#13949 = CARTESIAN_POINT ( 'NONE',  ( -0.8244235255442939891, -0.5829339996946389935, 2.492493020344019872 ) ) ;
#13950 = ORIENTED_EDGE ( 'NONE', *, *, #14173, .T. ) ;
#13951 = CARTESIAN_POINT ( 'NONE',  ( -0.6493550500446439999, -5.586652542372879005, 2.437955526623099889 ) ) ;
#13952 = CARTESIAN_POINT ( 'NONE',  ( 2.543624461644950152, -3.896469987729531681, 5.457025951419980814 ) ) ;
#13953 = CARTESIAN_POINT ( 'NONE',  ( 6.502734858518770642E-16, 3.500000000000000000, 6.100000000000000533 ) ) ;
#13954 = CARTESIAN_POINT ( 'NONE',  ( -1.224086244040909488, -1.241605122864670285, 6.348185277745776567 ) ) ;
#13955 = DIRECTION ( 'NONE',  ( 0.7071067811865480168, 0.000000000000000000, 0.7071067811865470176 ) ) ;
#13956 = ORIENTED_EDGE ( 'NONE', *, *, #12918, .T. ) ;
#13957 = LINE ( 'NONE', #5534, #13861 ) ;
#13958 = CARTESIAN_POINT ( 'NONE',  ( -1.661700935788390066, -0.5625000000000000000, 3.038299064211610112 ) ) ;
#13959 = CARTESIAN_POINT ( 'NONE',  ( -2.062913653388399826, -3.217268751009200400, 5.832754583370829415 ) ) ;
#13960 = CARTESIAN_POINT ( 'NONE',  ( -1.000000000000000000, -5.000000000000000000, 3.299999999999999822 ) ) ;
#13961 = DIRECTION ( 'NONE',  ( 1.110223024625159992E-16, 0.000000000000000000, -1.000000000000000000 ) ) ;
#13962 = CARTESIAN_POINT ( 'NONE',  ( 2.519547246525509543, -5.059745762711855832, 3.866491354109194756 ) ) ;
#13963 = ORIENTED_EDGE ( 'NONE', *, *, #15506, .T. ) ;
#13964 = DIRECTION ( 'NONE',  ( 1.000000000000000000, 0.000000000000000000, 0.000000000000000000 ) ) ;
#13965 = CARTESIAN_POINT ( 'NONE',  ( 0.5999999999999999778, -7.347880794884110368E-17, 7.599999999999999645 ) ) ;
#13966 = ORIENTED_EDGE ( 'NONE', *, *, #14444, .T. ) ;
#13967 = EDGE_CURVE ( 'NONE', #6214, #8884, #1402, .T. ) ;
#13968 = CARTESIAN_POINT ( 'NONE',  ( 0.1768565782245979934, -3.752899381639830168, 2.353200596935780098 ) ) ;
#13969 = SURFACE_STYLE_FILL_AREA ( #2863 ) ;
#13970 = CARTESIAN_POINT ( 'NONE',  ( 1.661700935788380074, -5.037500000000000533, 3.038299064211610112 ) ) ;
#13971 = CARTESIAN_POINT ( 'NONE',  ( -2.500000000000000000, 4.700000000000000178, 1.600000000000000089 ) ) ;
#13972 = DIRECTION ( 'NONE',  ( 0.000000000000000000, 0.000000000000000000, -1.000000000000000000 ) ) ;
#13973 = CARTESIAN_POINT ( 'NONE',  ( -0.6864473529425049181, -4.591277760018209975, 6.951118770549909343 ) ) ;
#13974 = CARTESIAN_POINT ( 'NONE',  ( 0.5500000000000000444, 0.5999999999999999778, 3.299999999999999822 ) ) ;
#13975 = CARTESIAN_POINT ( 'NONE',  ( 0.5302109551885175742, -3.799475958216412153, 2.716624547488259989 ) ) ;
#13976 = CARTESIAN_POINT ( 'NONE',  ( -1.112838723655040107, -0.4735169491525429986, 6.773667561836210105 ) ) ;
#13977 = CARTESIAN_POINT ( 'NONE',  ( 1.850000000000000089, 11.25000000000000000, 7.700000000000000178 ) ) ;
#13978 = VERTEX_POINT ( 'NONE', #9834 ) ;
#13979 = CARTESIAN_POINT ( 'NONE',  ( -1.750000000000000000, 11.40000000000000036, 7.550000000000000711 ) ) ;
#13980 = ORIENTED_EDGE ( 'NONE', *, *, #10528, .T. ) ;
#13981 = SURFACE_STYLE_FILL_AREA ( #10843 ) ;
#13982 = EDGE_LOOP ( 'NONE', ( #16974, #11189, #2586, #9855 ) ) ;
#13983 = ORIENTED_EDGE ( 'NONE', *, *, #15317, .F. ) ;
#13984 = UNCERTAINTY_MEASURE_WITH_UNIT (LENGTH_MEASURE( 1.000000000000000082E-05 ), #312, 'distance_accuracy_value', 'NONE');
#13985 =( BOUNDED_SURFACE ( )  B_SPLINE_SURFACE ( 3, 3, ( 
 ( #8420, #9716, #5734, #18197, #2684, #7040, #8609 ),
 ( #18031, #9811, #13887, #8337, #2777, #2864, #1482 ),
 ( #2592, #9900, #8514, #4238, #6851, #9995, #14252 ),
 ( #11099, #89, #7139, #14057, #9622, #5460, #13970 ),
 ( #15659, #15469, #1203, #1291, #12497, #5377, #2967 ),
 ( #5553, #15282, #16746, #18111, #4059, #12582, #15383 ),
 ( #11199, #6934, #12684, #16842, #5, #5647, #11290 ) ),
 .UNSPECIFIED., .T., .F., .F. ) 
 B_SPLINE_SURFACE_WITH_KNOTS ( ( 4, 3, 4 ),
 ( 4, 1, 1, 1, 4 ),
 ( 0.000000000000000000, 3.141592653589790007, 6.283185307179590673 ),
 ( 0.000000000000000000, 0.3003308066894049833, 0.4325493167363730351, 0.5576349185191149527, 0.7853981633974479459 ),
 .UNSPECIFIED. ) 
 GEOMETRIC_REPRESENTATION_ITEM ( )  RATIONAL_B_SPLINE_SURFACE ( (
 ( 1.000000000000000000, 1.000000000000000000, 1.000000000000000000, 1.000000000000000000, 1.000000000000000000, 1.000000000000000000, 1.000000000000000000),
 ( 0.3333333333333329818, 0.3333333333333329818, 0.3333333333333329818, 0.3333333333333329818, 0.3333333333333329818, 0.3333333333333329818, 0.3333333333333329818),
 ( 0.3333333333333329818, 0.3333333333333329818, 0.3333333333333329818, 0.3333333333333329818, 0.3333333333333329818, 0.3333333333333329818, 0.3333333333333329818),
 ( 1.000000000000000000, 1.000000000000000000, 1.000000000000000000, 1.000000000000000000, 1.000000000000000000, 1.000000000000000000, 1.000000000000000000),
 ( 0.3333333333333329818, 0.3333333333333329818, 0.3333333333333329818, 0.3333333333333329818, 0.3333333333333329818, 0.3333333333333329818, 0.3333333333333329818),
 ( 0.3333333333333329818, 0.3333333333333329818, 0.3333333333333329818, 0.3333333333333329818, 0.3333333333333329818, 0.3333333333333329818, 0.3333333333333329818),
 ( 1.000000000000000000, 1.000000000000000000, 1.000000000000000000, 1.000000000000000000, 1.000000000000000000, 1.000000000000000000, 1.000000000000000000) ) ) 
 REPRESENTATION_ITEM ( '' )  SURFACE ( )  );
#13986 = VERTEX_POINT ( 'NONE', #12709 ) ;
#13987 = CARTESIAN_POINT ( 'NONE',  ( 0.5500000000000000444, 2.050000000000000266, 3.600000000000000089 ) ) ;
#13988 = CARTESIAN_POINT ( 'NONE',  ( 1.949083719010301197, -5.059745762711855832, 4.055210292801453953 ) ) ;
#13989 = FACE_OUTER_BOUND ( 'NONE', #10445, .T. ) ;
#13990 = CARTESIAN_POINT ( 'NONE',  ( 0.6500000000000000222, 3.050000000000000266, 3.200000000000000178 ) ) ;
#13991 = CARTESIAN_POINT ( 'NONE',  ( 1.250000000000000000, 0.5999999999999999778, 7.599999999999999645 ) ) ;
#13992 = CARTESIAN_POINT ( 'NONE',  ( 2.500000000000000000, 2.799999999999999822, 1.600000000000000089 ) ) ;
#13993 = CARTESIAN_POINT ( 'NONE',  ( 0.5921572875253799939, 3.050000000000000266, 1.600000000000000089 ) ) ;
#13994 = CARTESIAN_POINT ( 'NONE',  ( -1.003115764947269950, -1.493935417675869903, 6.828967930617589666 ) ) ;
#13995 = CARTESIAN_POINT ( 'NONE',  ( -2.039016451601939117, -3.011515032774579215, 4.939402908764104261 ) ) ;
#13996 = ADVANCED_FACE ( 'NONE', ( #12516 ), #18224, .F. ) ;
#13997 = CARTESIAN_POINT ( 'NONE',  ( -2.224278379903029901, -0.2091101694915259990, 5.468825643806110470 ) ) ;
#13998 = ORIENTED_EDGE ( 'NONE', *, *, #9982, .F. ) ;
#13999 = CARTESIAN_POINT ( 'NONE',  ( 2.253200202764420013, -0.3889830508474579895, 5.379408587037500133 ) ) ;
#14000 = EDGE_CURVE ( 'NONE', #14847, #11001, #11397, .T. ) ;
#14001 = EDGE_CURVE ( 'NONE', #5569, #9670, #13238, .T. ) ;
#14002 = DIRECTION ( 'NONE',  ( 6.123233995736759873E-17, -6.123233995736769734E-17, 1.000000000000000000 ) ) ;
#14003 = ORIENTED_EDGE ( 'NONE', *, *, #4380, .F. ) ;
#14004 = CARTESIAN_POINT ( 'NONE',  ( 2.345900685764729765, -0.07118644067796649211, 4.512231114381330066 ) ) ;
#14005 = DIRECTION ( 'NONE',  ( 2.467162276944790449E-16, 0.000000000000000000, 1.000000000000000000 ) ) ;
#14006 = CIRCLE ( 'NONE', #6021, 0.5000000000000000000 ) ;
#14007 = ORIENTED_EDGE ( 'NONE', *, *, #1890, .F. ) ;
#14008 = CARTESIAN_POINT ( 'NONE',  ( -2.500000000000000000, 2.000000000000000000, 1.600000000000000089 ) ) ;
#14009 = EDGE_LOOP ( 'NONE', ( #5540, #11867, #2062, #5198 ) ) ;
#14010 = CARTESIAN_POINT ( 'NONE',  ( 1.669205944673859854, -2.452596113855660676, 6.359065158982410537 ) ) ;
#14011 =( NAMED_UNIT ( * ) PLANE_ANGLE_UNIT ( ) SI_UNIT ( $, .RADIAN. ) );
#14012 = CARTESIAN_POINT ( 'NONE',  ( 0.3171869470818560743, -5.444279661016954819, 7.334814496515233095 ) ) ;
#14013 = VERTEX_POINT ( 'NONE', #17289 ) ;
#14014 = CARTESIAN_POINT ( 'NONE',  ( -1.800000000000000044, 11.40000000000000036, 7.550000000000000711 ) ) ;
#14015 = CARTESIAN_POINT ( 'NONE',  ( -1.580445181003969912, -0.5580508474576266753, 3.389704561770339630 ) ) ;
#14016 = ORIENTED_EDGE ( 'NONE', *, *, #5567, .T. ) ;
#14017 = PLANE ( 'NONE',  #13797 ) ;
#14018 = LINE ( 'NONE', #1334, #16777 ) ;
#14019 = PLANE ( 'NONE',  #12705 ) ;
#14020 = CARTESIAN_POINT ( 'NONE',  ( -1.945780800405131350, -4.688271789531334832, 4.045142061754299689 ) ) ;
#14022 = ADVANCED_FACE ( 'NONE', ( #4714 ), #7684, .T. ) ;
#14021 = PLANE ( 'NONE',  #7027 ) ;
#14023 = ORIENTED_EDGE ( 'NONE', *, *, #4267, .T. ) ;
#14024 = CARTESIAN_POINT ( 'NONE',  ( 0.1749999999999999889, 2.700000000000000178, 1.600000000000000089 ) ) ;
#14025 = CYLINDRICAL_SURFACE ( 'NONE', #9393, 1.000000000000000000 ) ;
#14026 = CARTESIAN_POINT ( 'NONE',  ( 1.846259792136599076, -0.3533898305084745561, 3.802221692020924415 ) ) ;
#14027 = CARTESIAN_POINT ( 'NONE',  ( 0.4722227023514015687, -3.477280798540335560, 2.088464165977070408 ) ) ;
#14028 = ORIENTED_EDGE ( 'NONE', *, *, #3238, .T. ) ;
#14029 = CARTESIAN_POINT ( 'NONE',  ( 1.899999999999999911, 8.500000000000000000, 0.6099999999999999867 ) ) ;
#14030 = CARTESIAN_POINT ( 'NONE',  ( -0.4649462444738060030, -5.251463457376920552, 2.383584851084299849 ) ) ;
#14031 = CARTESIAN_POINT ( 'NONE',  ( 0.05465110135556765225, -5.148728813559319661, 6.752241303418941243 ) ) ;
#14032 = ORIENTED_EDGE ( 'NONE', *, *, #8711, .T. ) ;
#14033 = CARTESIAN_POINT ( 'NONE',  ( 1.194742379459969861, -0.1245762711864410038, 6.727584234649758521 ) ) ;
#14034 = CARTESIAN_POINT ( 'NONE',  ( 1.661700935788380074, -5.337500000000000355, 3.038299064211610112 ) ) ;
#14035 = CARTESIAN_POINT ( 'NONE',  ( 1.850000000000000089, 11.25000000000000000, 7.649999999999999467 ) ) ;
#14036 = ORIENTED_EDGE ( 'NONE', *, *, #5628, .T. ) ;
#14037 = LINE ( 'NONE', #7279, #12627 ) ;
#14038 = CARTESIAN_POINT ( 'NONE',  ( -0.8189529353761560992, -1.777235753495300052, 2.493631540942749858 ) ) ;
#14039 = CARTESIAN_POINT ( 'NONE',  ( -1.250000000000000000, 7.799999999999999822, 5.100000000000000533 ) ) ;
#14040 = CARTESIAN_POINT ( 'NONE',  ( -2.231116159141639965, -4.688271789531330391, 3.951089877392499616 ) ) ;
#14042 = EDGE_CURVE ( 'NONE', #2436, #15551, #17477, .T. ) ;
#14041 = DIRECTION ( 'NONE',  ( -6.167905692361979821E-17, 0.000000000000000000, -1.000000000000000000 ) ) ;
#14043 = EDGE_LOOP ( 'NONE', ( #16422, #7479, #6690, #13052 ) ) ;
#14044 = CARTESIAN_POINT ( 'NONE',  ( 1.668798118857418133, -5.037502670768956747, 3.031201881142577381 ) ) ;
#14045 = CARTESIAN_POINT ( 'NONE',  ( -1.112838723655040107, -0.4735169491525429986, 6.773667561836210105 ) ) ;
#14046 = CARTESIAN_POINT ( 'NONE',  ( -2.036228139452650243, -3.473439922180369788, 3.519948877554409883 ) ) ;
#14047 = CARTESIAN_POINT ( 'NONE',  ( -1.750000000000000000, 0.5999999999999999778, 7.550000000000000711 ) ) ;
#14048 = CARTESIAN_POINT ( 'NONE',  ( 2.416676968769261080, -5.095338983050850423, 5.796598111919825769 ) ) ;
#14049 = ORIENTED_EDGE ( 'NONE', *, *, #9715, .T. ) ;
#14050 = ORIENTED_EDGE ( 'NONE', *, *, #10168, .F. ) ;
#14051 = DIRECTION ( 'NONE',  ( 0.000000000000000000, 0.000000000000000000, 1.000000000000000000 ) ) ;
#14052 = LINE ( 'NONE', #7990, #15658 ) ;
#14053 = B_SPLINE_CURVE_WITH_KNOTS ( 'NONE', 3,
 ( #8672, #1828, #1905, #13119, #6070, #13197, #6166 ),
 .UNSPECIFIED., .F., .F.,
 ( 4, 1, 1, 1, 4 ),
 ( 5.497787143782139729, 5.798117950472390092, 5.930336460519450625, 6.055422062302069364, 6.283185307179590673 ),
 .UNSPECIFIED. ) ;
#14054 = CARTESIAN_POINT ( 'NONE',  ( -2.500000000000000000, 10.00000000000000000, 1.600000000000000089 ) ) ;
#14055 = ORIENTED_EDGE ( 'NONE', *, *, #15760, .F. ) ;
#14056 = CARTESIAN_POINT ( 'NONE',  ( 0.8001094918299610503, -1.307629111369559949, 7.230402832373829192 ) ) ;
#14057 = CARTESIAN_POINT ( 'NONE',  ( 0.9866023595736967966, -5.020626044399130627, 2.560054107758459985 ) ) ;
#14058 = DIRECTION ( 'NONE',  ( -6.167905692361979821E-17, 0.000000000000000000, -1.000000000000000000 ) ) ;
#14060 = EDGE_CURVE ( 'NONE', #6586, #17492, #10448, .T. ) ;
#14059 = CARTESIAN_POINT ( 'NONE',  ( -1.899999999999999911, 10.00000000000000000, 0.5999999999999999778 ) ) ;
#14061 = CARTESIAN_POINT ( 'NONE',  ( 1.567709126316360058, -3.915917399657849796, 2.944712621036570166 ) ) ;
#14062 = CARTESIAN_POINT ( 'NONE',  ( 0.1749999999999999889, 8.200000000000001066, -3.200000000000000178 ) ) ;
#14063 = CARTESIAN_POINT ( 'NONE',  ( -1.698651900122509995, -3.193980462720909408, 5.853032334688971439 ) ) ;
#14064 = CARTESIAN_POINT ( 'NONE',  ( 0.2335786437626899970, 6.450000000000000178, 2.241421356237310203 ) ) ;
#14065 = ORIENTED_EDGE ( 'NONE', *, *, #4843, .F. ) ;
#14066 = CARTESIAN_POINT ( 'NONE',  ( -1.066267773695860122, -0.5741044150835525883, 2.929718414487351374 ) ) ;
#14067 = ORIENTED_EDGE ( 'NONE', *, *, #16421, .T. ) ;
#14068 = PRESENTATION_STYLE_ASSIGNMENT (( #15835 ) ) ;
#14069 = ORIENTED_EDGE ( 'NONE', *, *, #7274, .F. ) ;
#14070 = EDGE_LOOP ( 'NONE', ( #15592, #2023, #5768, #12738 ) ) ;
#14071 = CARTESIAN_POINT ( 'NONE',  ( -1.399999999999999911, -8.000000000000000000, 3.299999999999999822 ) ) ;
#14072 = CARTESIAN_POINT ( 'NONE',  ( 0.2453710345350221533, -5.144279661016955885, 6.738252723719333481 ) ) ;
#14073 = CARTESIAN_POINT ( 'NONE',  ( 1.449852972479971358, -2.010118636378181112, 2.477154964647140911 ) ) ;
#14074 = CARTESIAN_POINT ( 'NONE',  ( -0.9000000000000000222, 6.450000000000000178, 3.600000000000000089 ) ) ;
#14075 = CARTESIAN_POINT ( 'NONE',  ( 1.751366433340660000, -0.7186644140778950529, 2.939816763756370133 ) ) ;
#14076 = DIRECTION ( 'NONE',  ( 2.490091241227950223E-32, -1.233581138472399909E-16, 1.000000000000000000 ) ) ;
#14077 = DIRECTION ( 'NONE',  ( 1.400676323190716506E-30, -1.000000000000000000, 0.000000000000000000 ) ) ;
#14078 = VECTOR ( 'NONE', #5222, 1000.000000000000000 ) ;
#14079 = CARTESIAN_POINT ( 'NONE',  ( 2.500000000000000000, 4.700000000000000178, 1.600000000000000089 ) ) ;
#14080 = CARTESIAN_POINT ( 'NONE',  ( 2.169623098572349917, -2.658349832090280529, 5.611855963200990338 ) ) ;
#14081 = CARTESIAN_POINT ( 'NONE',  ( -1.259207372045990869, -3.267686203945749490, 3.078488779929933639 ) ) ;
#14082 = CARTESIAN_POINT ( 'NONE',  ( -0.4974685680287780354, -0.1601694915254240070, 7.000224381598740386 ) ) ;
#14083 = MANIFOLD_SOLID_BREP ( 'Stock-MAS-687-1', #197 ) ;
#14084 = CARTESIAN_POINT ( 'NONE',  ( -1.661700935788390066, -0.5625000000000000000, 3.038299064211610112 ) ) ;
#14085 = PLANE ( 'NONE',  #17701 ) ;
#14086 = ORIENTED_EDGE ( 'NONE', *, *, #8132, .F. ) ;
#14087 = CARTESIAN_POINT ( 'NONE',  ( -2.224278379903029901, -0.2091101694915259990, 5.468825643806110470 ) ) ;
#14088 = CARTESIAN_POINT ( 'NONE',  ( 0.1226612266411070129, -2.937809291549740021, 7.050255286338659388 ) ) ;
#14089 = ORIENTED_EDGE ( 'NONE', *, *, #4296, .F. ) ;
#14090 = VECTOR ( 'NONE', #4176, 1000.000000000000000 ) ;
#14091 = VECTOR ( 'NONE', #4261, 1000.000000000000000 ) ;
#14092 = AXIS2_PLACEMENT_3D ( 'NONE', #18285, #14662, #11537 ) ;
#14093 = ORIENTED_EDGE ( 'NONE', *, *, #14128, .F. ) ;
#14094 = CARTESIAN_POINT ( 'NONE',  ( 2.351999299633229956, -2.266289807549349611, 4.782734406438239994 ) ) ;
#14095 = SHAPE_REPRESENTATION_RELATIONSHIP ( 'NONE' , 'NONE' ,  #4513, #5334 ) ;
#14096 = CARTESIAN_POINT ( 'NONE',  ( -0.4360591020458099987, -5.591101694915249887, 2.387347919655840034 ) ) ;
#14097 = VECTOR ( 'NONE', #3560, 1000.000000000000000 ) ;
#14098 = ADVANCED_FACE ( 'NONE', ( #12971 ), #4615, .T. ) ;
#14099 = EDGE_LOOP ( 'NONE', ( #11439, #6649, #15573, #6555 ) ) ;
#14100 = CARTESIAN_POINT ( 'NONE',  ( 1.644832646965660006, -1.191187669928119863, 6.383232381746459794 ) ) ;
#14101 = EDGE_CURVE ( 'NONE', #9239, #6891, #14452, .T. ) ;
#14102 = AXIS2_PLACEMENT_3D ( 'NONE', #487, #406, #17319 ) ;
#14103 = CARTESIAN_POINT ( 'NONE',  ( -1.494593880360799432, -0.5610169491525425212, 3.295456077495951153 ) ) ;
#14104 = AXIS2_PLACEMENT_3D ( 'NONE', #11437, #5520, #8398 ) ;
#14105 = ORIENTED_EDGE ( 'NONE', *, *, #3843, .T. ) ;
#14106 = CARTESIAN_POINT ( 'NONE',  ( -0.1749999999999999889, 8.800000000000000711, 0.4000000000000000222 ) ) ;
#14107 = DIRECTION ( 'NONE',  ( 2.337311630789800155E-16, -1.000000000000000000, -1.168655815394900078E-16 ) ) ;
#14108 = CARTESIAN_POINT ( 'NONE',  ( 1.800000000000000044, 0.5999999999999999778, 7.550000000000000711 ) ) ;
#14109 = CARTESIAN_POINT ( 'NONE',  ( 1.893291846171430981, -2.658349832090279197, 5.493944474033856551 ) ) ;
#14110 = PLANE ( 'NONE',  #2888 ) ;
#14111 = CARTESIAN_POINT ( 'NONE',  ( 0.4917262214558945632, -0.3088983050847459166, 2.092115739186370948 ) ) ;
#14112 = VECTOR ( 'NONE', #6521, 1000.000000000000000 ) ;
#14113 = ORIENTED_EDGE ( 'NONE', *, *, #2940, .T. ) ;
#14114 = LINE ( 'NONE', #7100, #4212 ) ;
#14115 = AXIS2_PLACEMENT_3D ( 'NONE', #1225, #18129, #15678 ) ;
#14116 = CARTESIAN_POINT ( 'NONE',  ( -1.800000000000000044, 11.40000000000000036, 1.600000000000000089 ) ) ;
#14117 = CARTESIAN_POINT ( 'NONE',  ( -0.4339619423229766348, -0.4601694915254239682, 6.706578715862737461 ) ) ;
#14118 = VERTEX_POINT ( 'NONE', #13149 ) ;
#14119 = AXIS2_PLACEMENT_3D ( 'NONE', #6041, #13165, #11793 ) ;
#14120 = CARTESIAN_POINT ( 'NONE',  ( 3.673940397442050254E-17, 2.600000000000000089, 8.000000000000000000 ) ) ;
#14121 = CARTESIAN_POINT ( 'NONE',  ( -2.046424002475610404, -5.528813559322025561, 4.536201610417774255 ) ) ;
#14122 = VERTEX_POINT ( 'NONE', #2029 ) ;
#14123 = AXIS2_PLACEMENT_3D ( 'NONE', #11883, #10568, #14842 ) ;
#14124 = EDGE_CURVE ( 'NONE', #14130, #16733, #13328, .T. ) ;
#14125 = CARTESIAN_POINT ( 'NONE',  ( 0.6493550500446279017, -0.01334745762711889855, 2.437955526623101665 ) ) ;
#14126 = CARTESIAN_POINT ( 'NONE',  ( 1.899999999999999911, 7.299999999999999822, 0.6099999999999999867 ) ) ;
#14127 = CARTESIAN_POINT ( 'NONE',  ( -2.200000000000000178, 4.053507564265650114E-17, 7.649999999999999467 ) ) ;
#14128 = EDGE_CURVE ( 'NONE', #2833, #7005, #8068, .T. ) ;
#14129 = ADVANCED_FACE ( 'NONE', ( #17841 ), #14815, .T. ) ;
#14130 = VERTEX_POINT ( 'NONE', #12317 ) ;
#14131 = CIRCLE ( 'NONE', #2906, 0.3500000000000001998 ) ;
#14132 = CARTESIAN_POINT ( 'NONE',  ( -1.149999999999999911, 6.447051294741199534, 6.942609934460510779 ) ) ;
#14133 = EDGE_CURVE ( 'NONE', #16005, #7550, #16475, .T. ) ;
#14134 = CARTESIAN_POINT ( 'NONE',  ( -0.6150581927481590938, -1.148451969711520082, 6.971662190339330323 ) ) ;
#14135 = EDGE_CURVE ( 'NONE', #2147, #17934, #13521, .T. ) ;
#14136 = DIRECTION ( 'NONE',  ( 0.000000000000000000, -1.000000000000000000, 0.000000000000000000 ) ) ;
#14137 = CARTESIAN_POINT ( 'NONE',  ( -2.350542563031990273, -4.595118636378179744, 4.817027120179790067 ) ) ;
#14139 = VECTOR ( 'NONE', #17985, 1000.000000000000000 ) ;
#14138 =( GEOMETRIC_REPRESENTATION_CONTEXT ( 3 ) GLOBAL_UNCERTAINTY_ASSIGNED_CONTEXT ( ( #12332 ) ) GLOBAL_UNIT_ASSIGNED_CONTEXT ( ( #9621, #8243, #1202 ) ) REPRESENTATION_CONTEXT ( 'NONE', 'WORKASPACE' ) );
#14140 = AXIS2_PLACEMENT_3D ( 'NONE', #12678, #11285, #14422 ) ;
#14141 = CYLINDRICAL_SURFACE ( 'NONE', #6398, 0.2999999999999999334 ) ;
#14142 = ORIENTED_EDGE ( 'NONE', *, *, #13240, .T. ) ;
#14143 = VECTOR ( 'NONE', #17397, 1000.000000000000000 ) ;
#14144 = AXIS2_PLACEMENT_3D ( 'NONE', #574, #6035, #4728 ) ;
#14145 = DIRECTION ( 'NONE',  ( 1.224646799147350002E-16, -1.000000000000000000, -6.123233995736769734E-17 ) ) ;
#14146 = CARTESIAN_POINT ( 'NONE',  ( 1.800129581279440893, -0.3355932203389832558, 2.750028594811110061 ) ) ;
#14147 = CARTESIAN_POINT ( 'NONE',  ( 0.1768565782245979934, -3.752899381639830168, 2.353200596935780098 ) ) ;
#14148 = PLANE ( 'NONE',  #8667 ) ;
#14149 = DIRECTION ( 'NONE',  ( 0.2800000000000002487, -6.217248937900882148E-17, -0.9599999999999998535 ) ) ;
#14150 = CARTESIAN_POINT ( 'NONE',  ( -0.2469343877495291661, -5.595550847457635868, 2.057675570509529539 ) ) ;
#14151 = ORIENTED_EDGE ( 'NONE', *, *, #13823, .F. ) ;
#14152 = ORIENTED_EDGE ( 'NONE', *, *, #6641, .F. ) ;
#14153 = CARTESIAN_POINT ( 'NONE',  ( 0.5372984490435490645, 4.599999999999999645, 8.300000000000000711 ) ) ;
#14154 =( NAMED_UNIT ( * ) PLANE_ANGLE_UNIT ( ) SI_UNIT ( $, .RADIAN. ) );
#14155 = VECTOR ( 'NONE', #1360, 1000.000000000000000 ) ;
#14156 = LINE ( 'NONE', #1477, #5866 ) ;
#14157 = VECTOR ( 'NONE', #13144, 1000.000000000000000 ) ;
#14158 = CIRCLE ( 'NONE', #14102, 0.5999999999999998668 ) ;
#14159 = ADVANCED_FACE ( 'NONE', ( #2324 ), #17938, .T. ) ;
#14160 = ORIENTED_EDGE ( 'NONE', *, *, #12878, .F. ) ;
#14161 = CARTESIAN_POINT ( 'NONE',  ( -2.161802606005209793, -5.010466949207389220, 3.769755311421840283 ) ) ;
#14162 = AXIS2_PLACEMENT_3D ( 'NONE', #5492, #11135, #5952 ) ;
#14163 = CARTESIAN_POINT ( 'NONE',  ( 1.475946938622679783, -0.7471169921413568504, 2.482078242844649729 ) ) ;
#14164 = LINE ( 'NONE', #1570, #15011 ) ;
#14165 = CARTESIAN_POINT ( 'NONE',  ( 1.899999999999999911, 11.40000000000000036, 1.600000000000000089 ) ) ;
#14166 = CARTESIAN_POINT ( 'NONE',  ( 2.349129089426440054, -0.7059744922340409623, 4.842612091679070474 ) ) ;
#14167 = CARTESIAN_POINT ( 'NONE',  ( 1.250000000000000000, 6.144112549695430303, 5.100000000000000533 ) ) ;
#14168 = CARTESIAN_POINT ( 'NONE',  ( -2.137408332595969629, -3.450151633892079683, 3.714996798363980002 ) ) ;
#14169 = AXIS2_PLACEMENT_3D ( 'NONE', #13594, #6344, #4866 ) ;
#14170 = CARTESIAN_POINT ( 'NONE',  ( 1.899999999999999911, 10.00000000000000000, 1.600000000000000089 ) ) ;
#14171 = CARTESIAN_POINT ( 'NONE',  ( -0.4625564304287554940, -3.007674156414608557, 6.700235833919871986 ) ) ;
#14172 = PLANE ( 'NONE',  #9698 ) ;
#14173 = EDGE_CURVE ( 'NONE', #1298, #14614, #17012, .T. ) ;
#14174 = LINE ( 'NONE', #14437, #3193 ) ;
#14175 = ORIENTED_EDGE ( 'NONE', *, *, #16496, .F. ) ;
#14176 = CARTESIAN_POINT ( 'NONE',  ( -0.7197963925281907205, -0.5829339996946386604, 2.774540890140321014 ) ) ;
#14177 = VERTEX_POINT ( 'NONE', #4153 ) ;
#14178 = DIRECTION ( 'NONE',  ( 1.000000000000000000, 0.000000000000000000, 0.000000000000000000 ) ) ;
#14179 = DIRECTION ( 'NONE',  ( 0.000000000000000000, 0.000000000000000000, 1.000000000000000000 ) ) ;
#14180 = EDGE_CURVE ( 'NONE', #1059, #9279, #14164, .T. ) ;
#14181 = ORIENTED_EDGE ( 'NONE', *, *, #16621, .T. ) ;
#14182 = CARTESIAN_POINT ( 'NONE',  ( -1.800000000000000044, 11.40000000000000036, 7.649999999999999467 ) ) ;
#14183 = EDGE_CURVE ( 'NONE', #404, #9178, #11377, .T. ) ;
#14184 = ORIENTED_EDGE ( 'NONE', *, *, #7143, .T. ) ;
#14185 = VECTOR ( 'NONE', #52, 1000.000000000000000 ) ;
#14186 = CARTESIAN_POINT ( 'NONE',  ( 2.030998484741458832, -5.081991525423726230, 4.999543428097175557 ) ) ;
#14187 = CARTESIAN_POINT ( 'NONE',  ( 2.409576349373750315, -2.149848366107909303, 3.587770028483080242 ) ) ;
#14188 = CARTESIAN_POINT ( 'NONE',  ( -1.899999999999999911, 0.7211102550927970256, 4.000000000000000000 ) ) ;
#14189 = DIRECTION ( 'NONE',  ( 2.537652627714639929E-16, 1.000000000000000000, -8.458842092382139670E-17 ) ) ;
#14190 = CARTESIAN_POINT ( 'NONE',  ( -1.149999999999999911, 6.472933199251450276, 6.846017351831609865 ) ) ;
#14191 = LINE ( 'NONE', #11124, #13230 ) ;
#14192 = LINE ( 'NONE', #17292, #4981 ) ;
#14193 = CARTESIAN_POINT ( 'NONE',  ( -2.137408332595969629, -3.450151633892079683, 3.714996798363980002 ) ) ;
#14194 = CARTESIAN_POINT ( 'NONE',  ( 1.798783563193339985, -2.382731248990799244, 5.689585537188965425 ) ) ;
#14195 = CARTESIAN_POINT ( 'NONE',  ( -2.155845792290839835, -0.2447033898305089883, 3.756158857535780271 ) ) ;
#14196 = FACE_OUTER_BOUND ( 'NONE', #13937, .T. ) ;
#14197 = CARTESIAN_POINT ( 'NONE',  ( -1.800000000000000044, 7.799999999999999822, 1.600000000000000089 ) ) ;
#14198 = EDGE_LOOP ( 'NONE', ( #14341, #10119, #17118, #8795 ) ) ;
#14199 = CARTESIAN_POINT ( 'NONE',  ( -2.234315482767910144, -0.2402542372881359967, 3.960850823455329905 ) ) ;
#14200 = CARTESIAN_POINT ( 'NONE',  ( 0.3413183941262679655, -2.914521003261450360, 7.028571974690709823 ) ) ;
#14201 = ORIENTED_EDGE ( 'NONE', *, *, #2191, .F. ) ;
#14202 = DIRECTION ( 'NONE',  ( 0.000000000000000000, 0.000000000000000000, -1.000000000000000000 ) ) ;
#14203 = VERTEX_POINT ( 'NONE', #8244 ) ;
#14204 = CARTESIAN_POINT ( 'NONE',  ( 1.465095039565329715, -2.033406924666470328, 2.858195935359850726 ) ) ;
#14205 = APPLICATION_PROTOCOL_DEFINITION ( 'draft international standard', 'automotive_design', 1998, #10890 ) ;
#14206 = CARTESIAN_POINT ( 'NONE',  ( -2.638803263991410741, -5.519915254237295343, 4.982085668537435730 ) ) ;
#14207 = ORIENTED_EDGE ( 'NONE', *, *, #8347, .F. ) ;
#14208 = CARTESIAN_POINT ( 'NONE',  ( -1.854177340199669954, -1.610376859117309989, 6.149404042554720284 ) ) ;
#14209 = VECTOR ( 'NONE', #7738, 1000.000000000000000 ) ;
#14210 = CARTESIAN_POINT ( 'NONE',  ( 0.6493550500446280127, -0.3133474576271190193, 2.437955526623099889 ) ) ;
#14211 = ORIENTED_EDGE ( 'NONE', *, *, #11988, .T. ) ;
#14212 = FACE_OUTER_BOUND ( 'NONE', #13451, .T. ) ;
#14213 = DIRECTION ( 'NONE',  ( -2.917038411497409743E-62, -1.000000000000000000, 1.836189155707839943E-31 ) ) ;
#14214 = CARTESIAN_POINT ( 'NONE',  ( -0.7368491673940088527, -2.076142624883081211, 2.783765372628170809 ) ) ;
#14215 = LINE ( 'NONE', #10048, #8800 ) ;
#14216 = CARTESIAN_POINT ( 'NONE',  ( 2.130266475405040882, -0.3444915254237289615, 3.117337770017949428 ) ) ;
#14217 = ORIENTED_EDGE ( 'NONE', *, *, #11893, .T. ) ;
#14218 = CARTESIAN_POINT ( 'NONE',  ( -0.4649462444738060030, -5.251463457376920552, 2.383584851084299849 ) ) ;
#14219 = DIRECTION ( 'NONE',  ( -1.000000000000000000, 6.659085919832825627E-16, 0.000000000000000000 ) ) ;
#14220 = ADVANCED_FACE ( 'NONE', ( #11015 ), #13985, .T. ) ;
#14221 = ORIENTED_EDGE ( 'NONE', *, *, #15584, .F. ) ;
#14222 = VECTOR ( 'NONE', #17006, 1000.000000000000000 ) ;
#14223 = DIRECTION ( 'NONE',  ( 3.749399456654639914E-33, 1.000000000000000000, 6.123233995736769734E-17 ) ) ;
#14224 = CARTESIAN_POINT ( 'NONE',  ( -1.202278654260740876, -5.479872881355935199, 6.364093491318035589 ) ) ;
#14225 = CARTESIAN_POINT ( 'NONE',  ( 0.5500000000000000444, 7.799999999999999822, 3.600000000000000089 ) ) ;
#14226 = CARTESIAN_POINT ( 'NONE',  ( 0.06264882350516240428, -5.448728813559320372, 7.052569299041220319 ) ) ;
#14227 = DIRECTION ( 'NONE',  ( -1.000000000000000000, 0.000000000000000000, 0.000000000000000000 ) ) ;
#14228 = ORIENTED_EDGE ( 'NONE', *, *, #8689, .F. ) ;
#14229 = CARTESIAN_POINT ( 'NONE',  ( -0.4005155088301869948, -1.125163681423230200, 7.019123328904779413 ) ) ;
#14230 = CARTESIAN_POINT ( 'NONE',  ( 1.836970198721020197E-17, 2.600000000000000089, 7.700000000000000178 ) ) ;
#14231 = VECTOR ( 'NONE', #3618, 1000.000000000000000 ) ;
#14232 = CARTESIAN_POINT ( 'NONE',  ( 1.951270856817530319, -2.336154672414218592, 5.338313313320885989 ) ) ;
#14233 = DIRECTION ( 'NONE',  ( 0.000000000000000000, 1.000000000000000000, 0.000000000000000000 ) ) ;
#14234 = ADVANCED_FACE ( 'NONE', ( #3123 ), #10346, .T. ) ;
#14235 = ORIENTED_EDGE ( 'NONE', *, *, #8407, .F. ) ;
#14236 = EDGE_CURVE ( 'NONE', #11589, #6491, #7484, .T. ) ;
#14237 = CARTESIAN_POINT ( 'NONE',  ( -2.500000000000000000, 11.25000000000000000, 7.649999999999999467 ) ) ;
#14238 = CARTESIAN_POINT ( 'NONE',  ( -1.873832970144350130, -0.5625000000000005551, 2.826167029855650270 ) ) ;
#14239 = ADVANCED_FACE ( 'NONE', ( #14688 ), #6084, .T. ) ;
#14240 = CARTESIAN_POINT ( 'NONE',  ( 1.021156010535390068, -3.846052534792979927, 2.579625955254269964 ) ) ;
#14241 = LINE ( 'NONE', #5806, #6889 ) ;
#14242 = EDGE_CURVE ( 'NONE', #14289, #6043, #14520, .T. ) ;
#14243 = CARTESIAN_POINT ( 'NONE',  ( -2.616666666666669805, 1.330536610280860259E-16, 4.000000000000000000 ) ) ;
#14244 = CARTESIAN_POINT ( 'NONE',  ( -2.484260633728970546, -5.242161016949150820, 3.766563288620799366 ) ) ;
#14245 = EDGE_LOOP ( 'NONE', ( #8621, #17451, #14201, #10565 ) ) ;
#14246 = ORIENTED_EDGE ( 'NONE', *, *, #17482, .F. ) ;
#14247 = CARTESIAN_POINT ( 'NONE',  ( -1.889104232906368974, -5.255508474576268796, 3.296507079072530377 ) ) ;
#14248 = CARTESIAN_POINT ( 'NONE',  ( -0.1749999999999999889, 6.799999999999999822, 1.600000000000000089 ) ) ;
#14249 = ORIENTED_EDGE ( 'NONE', *, *, #8601, .F. ) ;
#14250 = CARTESIAN_POINT ( 'NONE',  ( 2.185196738168471153, -0.8418633456037974971, 3.194002352996649474 ) ) ;
#14251 = CARTESIAN_POINT ( 'NONE',  ( 0.8675710780368863784, -0.4076464065212254684, 2.836323152971460981 ) ) ;
#14252 = CARTESIAN_POINT ( 'NONE',  ( 1.873832970144350130, -5.037500000000000533, 2.826167029855650270 ) ) ;
#14253 = CARTESIAN_POINT ( 'NONE',  ( 5.709718412357949331E-16, 4.000000000000000000, 6.100000000000000533 ) ) ;
#14254 = CARTESIAN_POINT ( 'NONE',  ( -2.301223891756910334, -2.988226744486289999, 5.193066210047999398 ) ) ;
#14255 = FACE_OUTER_BOUND ( 'NONE', #8654, .T. ) ;
#14256 = CARTESIAN_POINT ( 'NONE',  ( -1.626408692231610109, -4.707719201459649838, 6.401040991074980369 ) ) ;
#14257 = FACE_OUTER_BOUND ( 'NONE', #4962, .T. ) ;
#14258 = CARTESIAN_POINT ( 'NONE',  ( 2.043688444617268729, -4.102223705964154199, 4.504451070148833836 ) ) ;
#14259 = EDGE_CURVE ( 'NONE', #11828, #9567, #15914, .T. ) ;
#14260 = CARTESIAN_POINT ( 'NONE',  ( -0.5999999999999999778, 10.80000000000000071, 7.700000000000000178 ) ) ;
#14261 = CARTESIAN_POINT ( 'NONE',  ( 1.889104232906359870, -0.3444915254237289615, 3.296507079072520163 ) ) ;
#14262 = VERTEX_POINT ( 'NONE', #7567 ) ;
#14263 = DIRECTION ( 'NONE',  ( 0.000000000000000000, 0.000000000000000000, 1.000000000000000000 ) ) ;
#14264 = ORIENTED_EDGE ( 'NONE', *, *, #5312, .T. ) ;
#14265 = CARTESIAN_POINT ( 'NONE',  ( 1.000000000000002220, 9.099999999999999645, 7.700000000000000178 ) ) ;
#14266 = EDGE_LOOP ( 'NONE', ( #3446, #10762, #7173, #14093 ) ) ;
#14267 = LINE ( 'NONE', #16943, #12958 ) ;
#14268 = ORIENTED_EDGE ( 'NONE', *, *, #9832, .T. ) ;
#14269 = CARTESIAN_POINT ( 'NONE',  ( 0.9707742057416334225, -5.426483050847465073, 6.508944043303927174 ) ) ;
#14270 = EDGE_CURVE ( 'NONE', #9094, #7523, #11469, .T. ) ;
#14271 = DIRECTION ( 'NONE',  ( 1.000000000000000000, 0.000000000000000000, 0.000000000000000000 ) ) ;
#14272 = CARTESIAN_POINT ( 'NONE',  ( 1.899999999999999911, 11.15000000000000036, 1.600000000000000089 ) ) ;
#14273 = DIRECTION ( 'NONE',  ( 0.000000000000000000, -1.000000000000000000, 0.000000000000000000 ) ) ;
#14274 = LINE ( 'NONE', #15579, #8160 ) ;
#14275 = CARTESIAN_POINT ( 'NONE',  ( 2.500000000000000000, 11.15000000000000036, 1.600000000000000089 ) ) ;
#14276 = LINE ( 'NONE', #12884, #9724 ) ;
#14277 = EDGE_CURVE ( 'NONE', #10849, #9615, #15819, .T. ) ;
#14278 = CARTESIAN_POINT ( 'NONE',  ( 0.4539185741479240255, -2.215872354612800521, 2.390735265170440105 ) ) ;
#14279 = CARTESIAN_POINT ( 'NONE',  ( -1.404946080800599351, -3.244397915657463827, 3.202993536195951840 ) ) ;
#14280 = CARTESIAN_POINT ( 'NONE',  ( -2.234315482767910144, -0.2402542372881359967, 3.960850823455329905 ) ) ;
#14281 = EDGE_CURVE ( 'NONE', #490, #5888, #10245, .T. ) ;
#14282 = VECTOR ( 'NONE', #4393, 1000.000000000000000 ) ;
#14283 = CARTESIAN_POINT ( 'NONE',  ( 1.800000000000000044, 11.29999999999999893, 1.600000000000000089 ) ) ;
#14284 = CARTESIAN_POINT ( 'NONE',  ( -1.795861365445549973, -0.5491525423728815802, 3.705232155007899930 ) ) ;
#14285 = LINE ( 'NONE', #1605, #17407 ) ;
#14286 = ORIENTED_EDGE ( 'NONE', *, *, #18165, .F. ) ;
#14287 = CARTESIAN_POINT ( 'NONE',  ( 2.306642602145299925, -0.08453389830508530045, 5.166805192608480368 ) ) ;
#14288 = CARTESIAN_POINT ( 'NONE',  ( 2.322440385110930094, -2.518620102360550117, 4.319189883157390497 ) ) ;
#14289 = VERTEX_POINT ( 'NONE', #17104 ) ;
#14290 = ORIENTED_EDGE ( 'NONE', *, *, #12654, .T. ) ;
#14291 = CARTESIAN_POINT ( 'NONE',  ( 1.381042549632459426, -4.059488005747550865, 6.605640880016109051 ) ) ;
#14292 = DIRECTION ( 'NONE',  ( 1.000000000000000000, 0.000000000000000000, 0.000000000000000000 ) ) ;
#14293 = CARTESIAN_POINT ( 'NONE',  ( -0.9002849211310044453, -5.466525423728811006, 7.196465912290821443 ) ) ;
#14294 = VERTEX_POINT ( 'NONE', #8775 ) ;
#14295 = CARTESIAN_POINT ( 'NONE',  ( -1.289141334274979789, -0.4824152542372879826, 6.297747079672432413 ) ) ;
#14296 = ORIENTED_EDGE ( 'NONE', *, *, #4216, .T. ) ;
#14297 = PLANE ( 'NONE',  #5526 ) ;
#14298 = CARTESIAN_POINT ( 'NONE',  ( 1.250000000000000000, 6.144112549695419645, 6.100000000000000533 ) ) ;
#14299 = CARTESIAN_POINT ( 'NONE',  ( -0.6470883152343470668, -3.030962444702889780, 6.648378442427256729 ) ) ;
#14300 = VERTEX_POINT ( 'NONE', #11837 ) ;
#14301 = CARTESIAN_POINT ( 'NONE',  ( 1.600000000000000089, -1.127398508120030014E-17, 7.649999999999999467 ) ) ;
#14302 = AXIS2_PLACEMENT_3D ( 'NONE', #15671, #7057, #4074 ) ;
#14303 = CARTESIAN_POINT ( 'NONE',  ( -1.250000000000000000, 3.500000000000000000, 6.100000000000000533 ) ) ;
#14304 = CARTESIAN_POINT ( 'NONE',  ( 1.821706171509118954, -0.3978813559322044724, 5.646608543709396244 ) ) ;
#14305 = VECTOR ( 'NONE', #9020, 1000.000000000000000 ) ;
#14306 = ORIENTED_EDGE ( 'NONE', *, *, #18287, .F. ) ;
#14307 = CARTESIAN_POINT ( 'NONE',  ( 0.5500000000000000444, 0.5999999999999999778, 3.299999999999999822 ) ) ;
#14308 = CARTESIAN_POINT ( 'NONE',  ( -3.503171016405825766E-15, -5.600000000000000533, 2.649999999999998579 ) ) ;
#14309 = CARTESIAN_POINT ( 'NONE',  ( -1.641808337277739671, -0.1868644067796620678, 6.386111670537630403 ) ) ;
#14310 = CARTESIAN_POINT ( 'NONE',  ( 1.875000000000000000, -2.296212748401290437E-16, 7.700000000000000178 ) ) ;
#14311 = ORIENTED_EDGE ( 'NONE', *, *, #5359, .T. ) ;
#14312 = AXIS2_PLACEMENT_3D ( 'NONE', #1587, #5831, #14342 ) ;
#14313 = CARTESIAN_POINT ( 'NONE',  ( 1.626408692231650077, -0.8922807985403480302, 6.401040991074950171 ) ) ;
#14314 = CARTESIAN_POINT ( 'NONE',  ( 2.350000000000000089, -5.599999999999999645, 2.799999999999999822 ) ) ;
#14315 = CARTESIAN_POINT ( 'NONE',  ( -1.503314099254069447, -1.660794312053860633, 3.301805249040033363 ) ) ;
#14316 = DIRECTION ( 'NONE',  ( 0.000000000000000000, 0.000000000000000000, 1.000000000000000000 ) ) ;
#14317 = CARTESIAN_POINT ( 'NONE',  ( 11.62823001646920140, -1.904792371696999770E-14, 0.5999999999999559019 ) ) ;
#14318 = VERTEX_POINT ( 'NONE', #4428 ) ;
#14319 = CARTESIAN_POINT ( 'NONE',  ( 1.899999999999999911, 10.00000000000000000, 1.600000000000000089 ) ) ;
#14320 = CARTESIAN_POINT ( 'NONE',  ( 1.407651048079441525, -0.02669491525423760975, 2.450250343405061759 ) ) ;
#14321 = CARTESIAN_POINT ( 'NONE',  ( 2.190084968185480374, -4.032358841099290103, 3.838447030292440054 ) ) ;
#14322 = CARTESIAN_POINT ( 'NONE',  ( -1.399999999999999911, -7.000000000000000000, 3.299999999999999822 ) ) ;
#14323 = LINE ( 'NONE', #14415, #1799 ) ;
#14324 = CARTESIAN_POINT ( 'NONE',  ( -1.610878918935079840, -5.268855932203385883, 2.590989782159090815 ) ) ;
#14325 = VERTEX_POINT ( 'NONE', #16092 ) ;
#14326 = ORIENTED_EDGE ( 'NONE', *, *, #9253, .T. ) ;
#14327 = CARTESIAN_POINT ( 'NONE',  ( -1.057242234132099723, -5.277754237288138306, 2.597442975781531160 ) ) ;
#14328 = CARTESIAN_POINT ( 'NONE',  ( 1.646397141422329957, -0.7952877538855639417, 3.035510168540480169 ) ) ;
#14329 = VERTEX_POINT ( 'NONE', #13132 ) ;
#14330 = CARTESIAN_POINT ( 'NONE',  ( -1.930452136971070987, -1.587088570829020551, 6.521117305355617511 ) ) ;
#14331 = EDGE_CURVE ( 'NONE', #16312, #16352, #10088, .T. ) ;
#14332 = CARTESIAN_POINT ( 'NONE',  ( 0.2451610102875899921, -0.3251990024832500104, 2.350791033861340029 ) ) ;
#14333 = CARTESIAN_POINT ( 'NONE',  ( -1.600000000000000089, 1.602906964449920292E-16, 7.649999999999999467 ) ) ;
#14334 = CARTESIAN_POINT ( 'NONE',  ( 1.097561405233190124, -1.986830348089889897, 2.618148744692249785 ) ) ;
#14335 = EDGE_CURVE ( 'NONE', #2390, #11460, #9033, .T. ) ;
#14336 = CARTESIAN_POINT ( 'NONE',  ( -0.5500000000000000444, 7.799999999999999822, 1.600000000000000089 ) ) ;
#14337 = CARTESIAN_POINT ( 'NONE',  ( -2.556942001999829905, -1.843259742000191048, 3.989253004641622358 ) ) ;
#14338 = CARTESIAN_POINT ( 'NONE',  ( -0.6500000000000000222, 6.450000000000000178, 3.200000000000000178 ) ) ;
#14339 = CARTESIAN_POINT ( 'NONE',  ( -1.549925137359298599, -4.731007489747939054, 6.046340934239856857 ) ) ;
#14340 = PLANE ( 'NONE',  #11232 ) ;
#14341 = ORIENTED_EDGE ( 'NONE', *, *, #10357, .T. ) ;
#14342 = DIRECTION ( 'NONE',  ( 0.7071067811865466846, 0.000000000000000000, -0.7071067811865483499 ) ) ;
#14343 = ORIENTED_EDGE ( 'NONE', *, *, #5653, .T. ) ;
#14344 = CARTESIAN_POINT ( 'NONE',  ( -1.899999999999999911, 2.799999999999999822, 1.600000000000000089 ) ) ;
#14345 = EDGE_CURVE ( 'NONE', #15079, #1993, #4509, .T. ) ;
#14346 = ORIENTED_EDGE ( 'NONE', *, *, #14472, .F. ) ;
#14347 = CARTESIAN_POINT ( 'NONE',  ( 2.000624272291700034, -5.364194915254235418, 4.239366054775996595 ) ) ;
#14348 = CARTESIAN_POINT ( 'NONE',  ( 0.5921572875253799939, 6.450000000000000178, 1.600000000000000089 ) ) ;
#14349 = CARTESIAN_POINT ( 'NONE',  ( -2.653064503426820764, -3.034803321062870651, 4.766048721853594294 ) ) ;
#14350 = ADVANCED_FACE ( 'NONE', ( #15740 ), #14602, .T. ) ;
#14351 = SURFACE_STYLE_USAGE ( .BOTH. , #460 ) ;
#14352 = DIRECTION ( 'NONE',  ( 1.000000000000000000, 0.000000000000000000, 0.000000000000000000 ) ) ;
#14353 = EDGE_CURVE ( 'NONE', #6043, #9985, #3046, .T. ) ;
#14354 = CYLINDRICAL_SURFACE ( 'NONE', #10516, 0.1000000000000000472 ) ;
#14355 = CARTESIAN_POINT ( 'NONE',  ( -0.5230055860628765041, -5.251463457376924104, 2.087624054227240844 ) ) ;
#14356 = CYLINDRICAL_SURFACE ( 'NONE', #14408, 0.2000000000000000389 ) ;
#14357 = CARTESIAN_POINT ( 'NONE',  ( 0.6500000000000000222, 6.450000000000000178, 2.699264068711930253 ) ) ;
#14358 = CARTESIAN_POINT ( 'NONE',  ( 0.9719602541832789155, -2.844656138396589817, 6.843370931913530519 ) ) ;
#14359 = CARTESIAN_POINT ( 'NONE',  ( -1.683529720875190705, -4.455388906648449776, 5.875001924065656134 ) ) ;
#14360 = CARTESIAN_POINT ( 'NONE',  ( -1.112838723655040107, -0.1735169491525430097, 6.773667561836210105 ) ) ;
#14361 = DIRECTION ( 'NONE',  ( -1.734723475976809806E-16, 1.000000000000000000, 0.000000000000000000 ) ) ;
#14362 = DIRECTION ( 'NONE',  ( -1.000000000000000000, 0.000000000000000000, 4.318427418585891014E-15 ) ) ;
#14363 = VERTEX_POINT ( 'NONE', #11642 ) ;
#14364 = CARTESIAN_POINT ( 'NONE',  ( -0.02098813186357061100, -3.430704221963769562, 2.046196467083000403 ) ) ;
#14365 = EDGE_CURVE ( 'NONE', #2448, #8002, #17370, .T. ) ;
#14366 = CARTESIAN_POINT ( 'NONE',  ( -1.580445181003969912, -0.2580508474576271305, 3.389704561770339630 ) ) ;
#14367 = CARTESIAN_POINT ( 'NONE',  ( -2.199335452462570117, -1.866548030288480042, 3.862342996790939953 ) ) ;
#14368 = VERTEX_POINT ( 'NONE', #14333 ) ;
#14369 = ORIENTED_EDGE ( 'NONE', *, *, #11843, .F. ) ;
#14370 = CARTESIAN_POINT ( 'NONE',  ( 0.1569242594330759466, -4.199217735477281721, 7.048216443236287709 ) ) ;
#14371 = SHAPE_DEFINITION_REPRESENTATION ( #10818, #5932 ) ;
#14372 = CARTESIAN_POINT ( 'NONE',  ( 0.5609751937345880402, -5.139830508474575232, 7.293870047334757523 ) ) ;
#14373 = VECTOR ( 'NONE', #11560, 1000.000000000000000 ) ;
#14374 = EDGE_CURVE ( 'NONE', #7912, #3782, #8871, .T. ) ;
#14375 = ORIENTED_EDGE ( 'NONE', *, *, #10065, .F. ) ;
#14376 = DIRECTION ( 'NONE',  ( 1.000000000000000000, 1.480297366166879989E-15, -7.401486830834380223E-16 ) ) ;
#14377 = AXIS2_PLACEMENT_3D ( 'NONE', #4890, #15197, #6572 ) ;
#14378 = CARTESIAN_POINT ( 'NONE',  ( -2.051331987628511211, -0.5269067796610176213, 4.618035453557344461 ) ) ;
#14379 = ORIENTED_EDGE ( 'NONE', *, *, #13322, .T. ) ;
#14380 = CARTESIAN_POINT ( 'NONE',  ( 0.01333550863827670518, -2.169295778036230526, 2.647020699851690306 ) ) ;
#14381 = CARTESIAN_POINT ( 'NONE',  ( -2.500000000000000000, 2.799999999999999822, 0.6099999999999999867 ) ) ;
#14382 = ORIENTED_EDGE ( 'NONE', *, *, #4924, .F. ) ;
#14383 = CARTESIAN_POINT ( 'NONE',  ( 1.875000000000000000, 12.00000000000000000, 8.300000000000000711 ) ) ;
#14384 = CARTESIAN_POINT ( 'NONE',  ( 0.1749999999999999889, 9.299999999999998934, 1.600000000000000089 ) ) ;
#14385 = CARTESIAN_POINT ( 'NONE',  ( 1.901882987994760965, -0.3934322033898309257, 5.472995608211450147 ) ) ;
#14386 = CLOSED_SHELL ( 'NONE', ( #12292, #2094, #13680, #7821, #1669, #3052, #18255, #16279, #14098, #16781, #8693, #947, #17867, #10940, #15281, #5793, #6774, #5045, #9209, #1568 ) ) ;
#14387 = AXIS2_PLACEMENT_3D ( 'NONE', #11017, #14642, #5283 ) ;
#14388 = EDGE_CURVE ( 'NONE', #7262, #11698, #12658, .T. ) ;
#14389 = CARTESIAN_POINT ( 'NONE',  ( 1.655443486440889789, -5.337500988460059936, 3.044556513559109945 ) ) ;
#14390 = VERTEX_POINT ( 'NONE', #12949 ) ;
#14391 = LINE ( 'NONE', #14490, #8882 ) ;
#14392 = CARTESIAN_POINT ( 'NONE',  ( 2.332582362116870200, -5.368644067796609853, 4.387643303570810005 ) ) ;
#14393 = LINE ( 'NONE', #334, #7052 ) ;
#14394 = ADVANCED_FACE ( 'NONE', ( #11923 ), #13398, .T. ) ;
#14395 = LINE ( 'NONE', #14574, #9176 ) ;
#14396 = VECTOR ( 'NONE', #5434, 1000.000000000000114 ) ;
#14397 = EDGE_CURVE ( 'NONE', #16040, #13368, #7662, .T. ) ;
#14398 = VERTEX_POINT ( 'NONE', #9129 ) ;
#14399 = CARTESIAN_POINT ( 'NONE',  ( 2.500000000000000000, 1.148961478048660025E-16, 3.600000000000000089 ) ) ;
#14400 = CARTESIAN_POINT ( 'NONE',  ( -1.866416942370660026, -1.637506023765569863, 3.266391446483499994 ) ) ;
#14401 = VECTOR ( 'NONE', #1358, 1000.000000000000000 ) ;
#14402 = CARTESIAN_POINT ( 'NONE',  ( 2.500000000000000000, 0.8000000000000000444, -2.399999999999999911 ) ) ;
#14403 = VECTOR ( 'NONE', #1773, 1000.000000000000000 ) ;
#14404 = CARTESIAN_POINT ( 'NONE',  ( 0.2302241296434710538, -1.893677194936738806, 2.659926792304259990 ) ) ;
#14405 = DIRECTION ( 'NONE',  ( 1.224646799147350002E-16, -1.000000000000000000, -6.123233995736759873E-17 ) ) ;
#14406 = CARTESIAN_POINT ( 'NONE',  ( -1.899999999999999911, 4.700000000000000178, 1.600000000000000089 ) ) ;
#14407 = VERTEX_POINT ( 'NONE', #8048 ) ;
#14408 = AXIS2_PLACEMENT_3D ( 'NONE', #2895, #5675, #5760 ) ;
#14409 = AXIS2_PLACEMENT_3D ( 'NONE', #13327, #11663, #7419 ) ;
#14410 = DIRECTION ( 'NONE',  ( -4.485749594445070317E-16, 0.000000000000000000, -1.000000000000000000 ) ) ;
#14411 = CARTESIAN_POINT ( 'NONE',  ( 2.649108131072720695, -0.7059744922340407403, 4.859184807329644862 ) ) ;
#14412 = CARTESIAN_POINT ( 'NONE',  ( 1.973760952634081134, -0.04004237288135625850, 2.925986839873718992 ) ) ;
#14413 = CARTESIAN_POINT ( 'NONE',  ( -2.218077401483159683, -4.824160642901089702, 5.486688202856539576 ) ) ;
#14414 = LINE ( 'NONE', #13120, #7493 ) ;
#14415 = CARTESIAN_POINT ( 'NONE',  ( 1.875000000000000000, -2.296212748401290437E-16, 8.300000000000000711 ) ) ;
#14416 = CARTESIAN_POINT ( 'NONE',  ( -1.800129581279449775, -5.264406779661021218, 2.750028594811118943 ) ) ;
#14417 = ORIENTED_EDGE ( 'NONE', *, *, #205, .F. ) ;
#14418 = VECTOR ( 'NONE', #8110, 1000.000000000000000 ) ;
#14419 = VECTOR ( 'NONE', #8585, 1000.000000000000000 ) ;
#14420 = ORIENTED_EDGE ( 'NONE', *, *, #9373, .F. ) ;
#14421 = DIRECTION ( 'NONE',  ( -0.000000000000000000, 1.000000000000000000, 0.000000000000000000 ) ) ;
#14422 = DIRECTION ( 'NONE',  ( -0.9622640697945192834, -0.2721173643531198949, 0.000000000000000000 ) ) ;
#14423 = VERTEX_POINT ( 'NONE', #14786 ) ;
#14424 = CIRCLE ( 'NONE', #17959, 0.6100000000000000977 ) ;
#14425 = CARTESIAN_POINT ( 'NONE',  ( -2.334748642087669523, -4.940602084342530453, 4.403867486184871005 ) ) ;
#14426 = VECTOR ( 'NONE', #5679, 1000.000000000000114 ) ;
#14427 = CARTESIAN_POINT ( 'NONE',  ( -1.800000000000000044, 11.40000000000000036, 7.550000000000000711 ) ) ;
#14428 = DIRECTION ( 'NONE',  ( 0.000000000000000000, 0.000000000000000000, -1.000000000000000000 ) ) ;
#14429 = CARTESIAN_POINT ( 'NONE',  ( -1.214457691476030110, -1.730659176918720066, 2.684103622926369948 ) ) ;
#14430 = EDGE_CURVE ( 'NONE', #1528, #12922, #6634, .T. ) ;
#14431 = CARTESIAN_POINT ( 'NONE',  ( 0.5000000000000000000, 5.762741699796949391, 5.100000000000000533 ) ) ;
#14432 = VECTOR ( 'NONE', #18167, 1000.000000000000000 ) ;
#14433 = CARTESIAN_POINT ( 'NONE',  ( 2.426866425021050766, -0.8884399221803740421, 3.626019996130599665 ) ) ;
#14434 = AXIS2_PLACEMENT_3D ( 'NONE', #7647, #13291, #518 ) ;
#14435 = FACE_OUTER_BOUND ( 'NONE', #9431, .T. ) ;
#14436 = CARTESIAN_POINT ( 'NONE',  ( 1.704669856830330010, -0.8030495317899829510, 3.080704711052640210 ) ) ;
#14437 = CARTESIAN_POINT ( 'NONE',  ( 1.899999999999999911, 11.29999999999999893, 1.600000000000000089 ) ) ;
#14438 = VECTOR ( 'NONE', #16916, 1000.000000000000000 ) ;
#14439 = VECTOR ( 'NONE', #12030, 1000.000000000000000 ) ;
#14440 = PLANE ( 'NONE',  #16561 ) ;
#14441 = ORIENTED_EDGE ( 'NONE', *, *, #3034, .T. ) ;
#14442 = DIRECTION ( 'NONE',  ( 1.224646799147349263E-16, 0.000000000000000000, 1.000000000000000000 ) ) ;
#14443 = ORIENTED_EDGE ( 'NONE', *, *, #1576, .F. ) ;
#14444 = EDGE_CURVE ( 'NONE', #9205, #1235, #2296, .T. ) ;
#14445 = CARTESIAN_POINT ( 'NONE',  ( -1.875000000000000000, 0.7500000000000000000, 8.300000000000000711 ) ) ;
#14446 = AXIS2_PLACEMENT_3D ( 'NONE', #12557, #13948, #2556 ) ;
#14447 = VERTEX_POINT ( 'NONE', #2400 ) ;
#14448 = CARTESIAN_POINT ( 'NONE',  ( -0.6964468257805866980, -5.466525423728811006, 6.631228347243847132 ) ) ;
#14449 = CARTESIAN_POINT ( 'NONE',  ( -1.875000000000000000, 12.00000000000000000, 7.700000000000000178 ) ) ;
#14450 = CARTESIAN_POINT ( 'NONE',  ( -0.02098813186357061100, -3.430704221963769562, 2.046196467083000403 ) ) ;
#14451 = DIRECTION ( 'NONE',  ( -1.000000000000000000, 0.000000000000000000, 0.000000000000000000 ) ) ;
#14452 = LINE ( 'NONE', #3406, #12039 ) ;
#14453 = CIRCLE ( 'NONE', #7655, 0.5999999999999999778 ) ;
#14454 = DIRECTION ( 'NONE',  ( 0.000000000000000000, -1.000000000000000000, -6.167905692361979821E-17 ) ) ;
#14455 = AXIS2_PLACEMENT_3D ( 'NONE', #3247, #4359, #8632 ) ;
#14456 = CARTESIAN_POINT ( 'NONE',  ( 2.350542563031990273, -1.004881363621820123, 4.817027120179740329 ) ) ;
#14457 = CARTESIAN_POINT ( 'NONE',  ( -0.6914213562373099364, 6.450000000000000178, 2.557842712474620139 ) ) ;
#14458 = CARTESIAN_POINT ( 'NONE',  ( -2.326448859701059746, -3.380286769027220029, 4.344498395672320434 ) ) ;
#14459 = CARTESIAN_POINT ( 'NONE',  ( 1.353302556710500371, -4.036199717459260761, 6.243850391919140819 ) ) ;
#14460 = EDGE_CURVE ( 'NONE', #2692, #7150, #17630, .T. ) ;
#14461 = CARTESIAN_POINT ( 'NONE',  ( -2.616666666666669805, -2.774341069716839796E-16, 7.649999999999999467 ) ) ;
#14462 = PRODUCT_DEFINITION ( 'UNKNOWN', '', #12712, #1218 ) ;
#14463 = CARTESIAN_POINT ( 'NONE',  ( 1.899999999999999911, 7.299999999999999822, 0.5999999999999999778 ) ) ;
#14464 = VERTEX_POINT ( 'NONE', #997 ) ;
#14465 = CARTESIAN_POINT ( 'NONE',  ( 2.380466601827069262, -3.710163681423226389, 3.526759849567131955 ) ) ;
#14466 = EDGE_CURVE ( 'NONE', #1106, #14363, #15027, .T. ) ;
#14467 = CARTESIAN_POINT ( 'NONE',  ( -2.030998484741458832, -0.2180084745762719822, 4.999543428097190656 ) ) ;
#14468 = CARTESIAN_POINT ( 'NONE',  ( 1.611907055891590002, -2.355602084342530045, 2.985210995296850189 ) ) ;
#14469 = ORIENTED_EDGE ( 'NONE', *, *, #15724, .T. ) ;
#14470 = AXIS2_PLACEMENT_3D ( 'NONE', #12113, #5252, #9219 ) ;
#14471 = ORIENTED_EDGE ( 'NONE', *, *, #3866, .T. ) ;
#14472 = EDGE_CURVE ( 'NONE', #14776, #17593, #16743, .T. ) ;
#14473 = PLANE ( 'NONE',  #10899 ) ;
#14474 = VERTEX_POINT ( 'NONE', #713 ) ;
#14475 = CARTESIAN_POINT ( 'NONE',  ( 2.182690844914369599, -3.919758276017820453, 5.580117243900430068 ) ) ;
#14476 = EDGE_CURVE ( 'NONE', #11896, #4807, #2101, .T. ) ;
#14477 = CARTESIAN_POINT ( 'NONE',  ( -2.458531667407850563, -5.206567796610170440, 5.699238225248945966 ) ) ;
#14478 = ORIENTED_EDGE ( 'NONE', *, *, #15257, .T. ) ;
#14479 = DIRECTION ( 'NONE',  ( 3.652293603810800245E-15, 1.332267629550190018E-15, -1.000000000000000000 ) ) ;
#14480 = CARTESIAN_POINT ( 'NONE',  ( 0.3743405594629510280, -0.4423728813559330009, 7.023440622744399953 ) ) ;
#14481 = ORIENTED_EDGE ( 'NONE', *, *, #10271, .T. ) ;
#14482 = DIRECTION ( 'NONE',  ( 5.551115123125880521E-15, -1.000000000000000000, -6.055990775824630636E-30 ) ) ;
#14483 = VECTOR ( 'NONE', #10028, 1000.000000000000000 ) ;
#14484 = CARTESIAN_POINT ( 'NONE',  ( -1.454969160281959661, -3.147403886144331420, 6.148435909958226198 ) ) ;
#14485 = DIRECTION ( 'NONE',  ( -6.344131569286609929E-16, -1.000000000000000000, 1.586032892321649771E-16 ) ) ;
#14486 = ORIENTED_EDGE ( 'NONE', *, *, #2827, .F. ) ;
#14487 = DIRECTION ( 'NONE',  ( -1.000000000000000000, 0.000000000000000000, 0.000000000000000000 ) ) ;
#14488 = EDGE_CURVE ( 'NONE', #12005, #13844, #6347, .T. ) ;
#14489 = ORIENTED_EDGE ( 'NONE', *, *, #7447, .F. ) ;
#14490 = CARTESIAN_POINT ( 'NONE',  ( -1.399999999999999911, 6.400000000000000355, 7.700000000000000178 ) ) ;
#14491 = CARTESIAN_POINT ( 'NONE',  ( -1.846259792136611066, -5.546610169491530407, 3.802221692020929744 ) ) ;
#14492 = PRESENTATION_STYLE_ASSIGNMENT (( #10214 ) ) ;
#14493 = CARTESIAN_POINT ( 'NONE',  ( -3.108624468950439891E-15, -5.299999999999999822, 1.110223024625159893E-15 ) ) ;
#14494 = VECTOR ( 'NONE', #161, 1000.000000000000000 ) ;
#14495 = CARTESIAN_POINT ( 'NONE',  ( -2.327043743583479429, -3.217268751009201289, 5.975923629552665872 ) ) ;
#14496 = ORIENTED_EDGE ( 'NONE', *, *, #11416, .T. ) ;
#14497 = CARTESIAN_POINT ( 'NONE',  ( -1.902324933209429858, -3.197821339080880065, 3.314393441133570040 ) ) ;
#14498 = LINE ( 'NONE', #13110, #15322 ) ;
#14499 = CARTESIAN_POINT ( 'NONE',  ( -1.959085573314230055, -2.964938456198001671, 5.313910057793616026 ) ) ;
#14500 = CARTESIAN_POINT ( 'NONE',  ( -2.350000000000000089, -5.599999999999999645, 6.400000000000000355 ) ) ;
#14501 = LINE ( 'NONE', #11816, #10615 ) ;
#14502 = ORIENTED_EDGE ( 'NONE', *, *, #3366, .T. ) ;
#14503 = VECTOR ( 'NONE', #1830, 1000.000000000000227 ) ;
#14504 = EDGE_CURVE ( 'NONE', #6533, #10817, #10806, .T. ) ;
#14505 = CARTESIAN_POINT ( 'NONE',  ( -1.800000000000000044, 11.40000000000000036, 7.649999999999999467 ) ) ;
#14506 = CARTESIAN_POINT ( 'NONE',  ( -2.248786803694121428, -1.334758276017820267, 6.109280527266697014 ) ) ;
#14507 = CARTESIAN_POINT ( 'NONE',  ( 2.260890494820590124, -4.055647129387580208, 4.046455925041149371 ) ) ;
#14508 = CARTESIAN_POINT ( 'NONE',  ( -1.875000000000000000, 12.00000000000000000, 8.300000000000000711 ) ) ;
#14509 = PLANE ( 'NONE',  #7411 ) ;
#14510 = CARTESIAN_POINT ( 'NONE',  ( -2.386628511786350160, -5.246610169491530584, 3.539457309197792778 ) ) ;
#14511 = EDGE_LOOP ( 'NONE', ( #14811, #16983, #16026, #15877 ) ) ;
#14512 = EDGE_LOOP ( 'NONE', ( #14924, #17490, #11331, #3264 ) ) ;
#14513 = FACE_OUTER_BOUND ( 'NONE', #16551, .T. ) ;
#14514 = DIRECTION ( 'NONE',  ( 0.000000000000000000, -1.000000000000000000, 0.000000000000000000 ) ) ;
#14515 = ORIENTED_EDGE ( 'NONE', *, *, #15713, .F. ) ;
#14516 = VECTOR ( 'NONE', #2091, 1000.000000000000000 ) ;
#14517 = FACE_OUTER_BOUND ( 'NONE', #1359, .T. ) ;
#14518 = CARTESIAN_POINT ( 'NONE',  ( 2.653064503426820764, -2.565196678937129438, 4.766048721853534786 ) ) ;
#14519 = CARTESIAN_POINT ( 'NONE',  ( 0.009452110982655399438, -0.3001920447045380858, 2.050000000000001155 ) ) ;
#14520 = LINE ( 'NONE', #12859, #5232 ) ;
#14521 = CARTESIAN_POINT ( 'NONE',  ( -1.021156010535440029, -1.753947465207009948, 2.579625955254300163 ) ) ;
#14522 = DIRECTION ( 'NONE',  ( 0.000000000000000000, -1.000000000000000000, 0.000000000000000000 ) ) ;
#14523 = CARTESIAN_POINT ( 'NONE',  ( -2.235075160050040921, -1.633665147405598761, 6.130927224539796327 ) ) ;
#14524 = CARTESIAN_POINT ( 'NONE',  ( 4.225031457058369810E-16, 2.299999999999999822, 7.599999999999999645 ) ) ;
#14525 = LINE ( 'NONE', #4784, #10873 ) ;
#14526 = CARTESIAN_POINT ( 'NONE',  ( 0.7205524543785531977, -4.428259742000194343, 6.622421910798232503 ) ) ;
#14527 = FACE_OUTER_BOUND ( 'NONE', #5336, .T. ) ;
#14528 = VERTEX_POINT ( 'NONE', #3862 ) ;
#14529 = PLANE ( 'NONE',  #5445 ) ;
#14530 = ORIENTED_EDGE ( 'NONE', *, *, #15192, .F. ) ;
#14531 = CARTESIAN_POINT ( 'NONE',  ( -1.399999999999999911, -8.000000000000000000, 6.100000000000000533 ) ) ;
#14532 = LINE ( 'NONE', #10532, #16518 ) ;
#14533 = ADVANCED_FACE ( 'NONE', ( #16555 ), #3576, .F. ) ;
#14534 = ORIENTED_EDGE ( 'NONE', *, *, #9998, .F. ) ;
#14535 = CARTESIAN_POINT ( 'NONE',  ( -1.351903350398179438, -5.484322033898315851, 6.245004350000422200 ) ) ;
#14536 = LINE ( 'NONE', #13057, #16817 ) ;
#14537 = CARTESIAN_POINT ( 'NONE',  ( 2.329383452786330189, -1.028169651910100013, 5.035735636132829818 ) ) ;
#14538 = DIRECTION ( 'NONE',  ( 6.437450399132682577E-16, 1.000000000000000000, 0.000000000000000000 ) ) ;
#14539 = CARTESIAN_POINT ( 'NONE',  ( 2.155845792290829621, -5.355296610169490101, 3.756158857535770057 ) ) ;
#14540 = DIRECTION ( 'NONE',  ( -1.480297366166879989E-16, -5.921189464667500234E-16, 1.000000000000000000 ) ) ;
#14541 = CARTESIAN_POINT ( 'NONE',  ( 1.644832646965660006, -1.191187669928119863, 6.383232381746459794 ) ) ;
#14542 = CARTESIAN_POINT ( 'NONE',  ( 2.100188519621589922, -4.009070552810999999, 3.637948273607370275 ) ) ;
#14543 = CARTESIAN_POINT ( 'NONE',  ( -1.790316459643189972, -4.734848366107908824, 3.695177221627210074 ) ) ;
#14544 = CARTESIAN_POINT ( 'NONE',  ( -0.009452110982656868748, -5.299807955295460005, 2.350000000000000089 ) ) ;
#14545 = CARTESIAN_POINT ( 'NONE',  ( 1.899999999999999911, 2.481229107598859903E-16, -2.399999999999999911 ) ) ;
#14546 = VERTEX_POINT ( 'NONE', #13306 ) ;
#14547 = CARTESIAN_POINT ( 'NONE',  ( -1.562863241354461641, -0.1913135593220339215, 6.031217337312382298 ) ) ;
#14548 = CARTESIAN_POINT ( 'NONE',  ( 1.021156010535390068, -3.846052534792979927, 2.579625955254269964 ) ) ;
#14549 = ORIENTED_EDGE ( 'NONE', *, *, #129, .T. ) ;
#14550 = VECTOR ( 'NONE', #11145, 1000.000000000000000 ) ;
#14551 = VERTEX_POINT ( 'NONE', #3668 ) ;
#14552 = DIRECTION ( 'NONE',  ( -1.224646799147351975E-16, 1.000000000000000000, 6.123233995736759873E-17 ) ) ;
#14553 = ADVANCED_FACE ( 'NONE', ( #16178 ), #13493, .F. ) ;
#14554 = ORIENTED_EDGE ( 'NONE', *, *, #15815, .F. ) ;
#14555 = CARTESIAN_POINT ( 'NONE',  ( -2.145694642186068979, -4.501965483225029097, 5.666819626392590514 ) ) ;
#14556 = DIRECTION ( 'NONE',  ( 0.000000000000000000, 0.000000000000000000, 1.000000000000000000 ) ) ;
#14557 = CARTESIAN_POINT ( 'NONE',  ( -1.800129581279449775, -5.564406779661021041, 2.750028594811118943 ) ) ;
#14558 = CARTESIAN_POINT ( 'NONE',  ( -1.699999999999999956, 9.299999999999998934, 7.599999999999999645 ) ) ;
#14559 = CARTESIAN_POINT ( 'NONE',  ( 1.194742379459969861, -0.4245762711864409789, 6.727584234649759409 ) ) ;
#14560 = ORIENTED_EDGE ( 'NONE', *, *, #13766, .F. ) ;
#14561 = EDGE_CURVE ( 'NONE', #14614, #2121, #9223, .T. ) ;
#14562 = CARTESIAN_POINT ( 'NONE',  ( 1.899999999999999911, 10.00000000000000000, 1.600000000000000089 ) ) ;
#14563 = FACE_OUTER_BOUND ( 'NONE', #14769, .T. ) ;
#14564 = EDGE_CURVE ( 'NONE', #3610, #5685, #808, .T. ) ;
#14565 = CARTESIAN_POINT ( 'NONE',  ( -1.861802609626409089, -4.800872354612795156, 5.565212624397245733 ) ) ;
#14566 = EDGE_CURVE ( 'NONE', #18124, #5409, #17735, .T. ) ;
#14567 = CARTESIAN_POINT ( 'NONE',  ( -2.191755591049691532, -0.5536016949152540167, 3.203650300307721466 ) ) ;
#14568 = VERTEX_POINT ( 'NONE', #3763 ) ;
#14569 = FACE_OUTER_BOUND ( 'NONE', #17995, .T. ) ;
#14570 = ORIENTED_EDGE ( 'NONE', *, *, #3260, .F. ) ;
#14571 = CARTESIAN_POINT ( 'NONE',  ( 2.500000000000000000, 8.500000000000000000, 0.6099999999999999867 ) ) ;
#14572 = CARTESIAN_POINT ( 'NONE',  ( -1.707817112497179934, -5.488771186440679628, 6.319218296629480314 ) ) ;
#14573 = VECTOR ( 'NONE', #9888, 1000.000000000000000 ) ;
#14574 = CARTESIAN_POINT ( 'NONE',  ( -1.000000000000000000, -5.000000000000000000, 6.100000000000000533 ) ) ;
#14575 = CARTESIAN_POINT ( 'NONE',  ( 1.947945325730759292, -4.311818300558746486, 6.502393603230323116 ) ) ;
#14576 = ORIENTED_EDGE ( 'NONE', *, *, #6504, .T. ) ;
#14577 = ADVANCED_FACE ( 'NONE', ( #9425 ), #13689, .F. ) ;
#14578 =( BOUNDED_SURFACE ( )  B_SPLINE_SURFACE ( 3, 3, ( 
 ( #8311, #11165, #12833, #13949, #2836, #18276, #11265 ),
 ( #16814, #4128, #18168, #2755, #65, #147, #14752 ),
 ( #418, #1722, #3444, #15793, #17242, #8929, #4560 ),
 ( #9092, #4839, #7537, #7721, #6148, #10484, #10217 ),
 ( #2067, #13365, #6317, #11979, #17591, #3101, #8748 ),
 ( #7374, #17787, #17878, #8009, #2168, #9571, #5124 ),
 ( #9284, #964, #10870, #15054, #1057, #13456, #16328 ) ),
 .UNSPECIFIED., .T., .F., .F. ) 
 B_SPLINE_SURFACE_WITH_KNOTS ( ( 4, 3, 4 ),
 ( 4, 1, 1, 1, 4 ),
 ( 0.000000000000000000, 3.141592653589790007, 6.283185307179590673 ),
 ( 5.497787143782139729, 5.798117950472390092, 5.930336460519450625, 6.055422062302069364, 6.283185307179590673 ),
 .UNSPECIFIED. ) 
 GEOMETRIC_REPRESENTATION_ITEM ( )  RATIONAL_B_SPLINE_SURFACE ( (
 ( 1.000000000000000000, 1.000000000000000000, 1.000000000000000000, 1.000000000000000000, 1.000000000000000000, 1.000000000000000000, 1.000000000000000000),
 ( 0.3333333333333329818, 0.3333333333333329818, 0.3333333333333329818, 0.3333333333333329818, 0.3333333333333329818, 0.3333333333333329818, 0.3333333333333329818),
 ( 0.3333333333333329818, 0.3333333333333329818, 0.3333333333333329818, 0.3333333333333329818, 0.3333333333333329818, 0.3333333333333329818, 0.3333333333333329818),
 ( 1.000000000000000000, 1.000000000000000000, 1.000000000000000000, 1.000000000000000000, 1.000000000000000000, 1.000000000000000000, 1.000000000000000000),
 ( 0.3333333333333329818, 0.3333333333333329818, 0.3333333333333329818, 0.3333333333333329818, 0.3333333333333329818, 0.3333333333333329818, 0.3333333333333329818),
 ( 0.3333333333333329818, 0.3333333333333329818, 0.3333333333333329818, 0.3333333333333329818, 0.3333333333333329818, 0.3333333333333329818, 0.3333333333333329818),
 ( 1.000000000000000000, 1.000000000000000000, 1.000000000000000000, 1.000000000000000000, 1.000000000000000000, 1.000000000000000000, 1.000000000000000000) ) ) 
 REPRESENTATION_ITEM ( '' )  SURFACE ( )  );
#14579 = CARTESIAN_POINT ( 'NONE',  ( 1.145304265383909836, -2.522460978720529656, 6.755972720436079548 ) ) ;
#14580 = EDGE_CURVE ( 'NONE', #17990, #9201, #2563, .T. ) ;
#14581 = DIRECTION ( 'NONE',  ( 5.421010862427519212E-16, 1.000000000000000000, 0.000000000000000000 ) ) ;
#14582 = CARTESIAN_POINT ( 'NONE',  ( 0.3367924244280819934, 2.254758922476410188, 7.700000000000000178 ) ) ;
#14583 = CARTESIAN_POINT ( 'NONE',  ( 1.673492459604400961, -2.103271789531340641, 3.510746103527379702 ) ) ;
#14584 = VECTOR ( 'NONE', #519, 1000.000000000000000 ) ;
#14585 = ORIENTED_EDGE ( 'NONE', *, *, #12820, .T. ) ;
#14586 = DIRECTION ( 'NONE',  ( 1.000000000000000000, -1.480297366166869931E-15, 0.000000000000000000 ) ) ;
#14587 = CARTESIAN_POINT ( 'NONE',  ( 2.408279507600870950, -0.7991276453871939411, 5.815035204050346351 ) ) ;
#14588 = ORIENTED_EDGE ( 'NONE', *, *, #10639, .T. ) ;
#14589 = PLANE ( 'NONE',  #14434 ) ;
#14590 = DIRECTION ( 'NONE',  ( 0.000000000000000000, 0.2588190451025180749, -0.9659258262890690894 ) ) ;
#14591 = DIRECTION ( 'NONE',  ( 0.7071067811865480168, -0.7071067811865470176, 0.000000000000000000 ) ) ;
#14592 = CARTESIAN_POINT ( 'NONE',  ( 1.851400890972779045, -5.113135593220339281, 6.601359968904126241 ) ) ;
#14593 = VERTEX_POINT ( 'NONE', #9601 ) ;
#14594 = ORIENTED_EDGE ( 'NONE', *, *, #1887, .T. ) ;
#14595 = DIRECTION ( 'NONE',  ( 3.700743415417190112E-16, 1.000000000000000000, 1.268826313857319964E-16 ) ) ;
#14596 =( LENGTH_UNIT ( ) NAMED_UNIT ( * ) SI_UNIT ( .MILLI., .METRE. ) );
#14597 = CARTESIAN_POINT ( 'NONE',  ( 0.9000000000000000222, 6.450000000000000178, 3.600000000000000089 ) ) ;
#14598 = ORIENTED_EDGE ( 'NONE', *, *, #16944, .F. ) ;
#14599 = CARTESIAN_POINT ( 'NONE',  ( -1.597383073937548970, -2.006277760018210898, 2.580688553303291943 ) ) ;
#14600 = EDGE_CURVE ( 'NONE', #14177, #8965, #10559, .T. ) ;
#14601 = CARTESIAN_POINT ( 'NONE',  ( 0.009452110982655408111, -0.3001920447045370310, 2.350000000000000089 ) ) ;
#14602 = PLANE ( 'NONE',  #16187 ) ;
#14603 = CARTESIAN_POINT ( 'NONE',  ( -2.169623098572329933, -2.941650167909710234, 5.611855963201049846 ) ) ;
#14604 = CARTESIAN_POINT ( 'NONE',  ( 1.536215498768950027, -5.033893599512579975, 2.912754292501710474 ) ) ;
#14605 = CARTESIAN_POINT ( 'NONE',  ( 0.3162622016569809347, -1.354205687946139491, 7.334974746141788238 ) ) ;
#14606 = VECTOR ( 'NONE', #7857, 1000.000000000000000 ) ;
#14607 = CARTESIAN_POINT ( 'NONE',  ( 0.1749999999999999889, 7.900000000000000355, 0.5999999999999999778 ) ) ;
#14608 = CARTESIAN_POINT ( 'NONE',  ( 2.291237445532070094, -0.9350164987569499209, 4.162434510291790346 ) ) ;
#14609 = FACE_OUTER_BOUND ( 'NONE', #3197, .T. ) ;
#14610 = CARTESIAN_POINT ( 'NONE',  ( 2.088297318559229954, -0.3978813559322040283, 5.785136623276629919 ) ) ;
#14611 = PLANE ( 'NONE',  #3532 ) ;
#14612 = ORIENTED_EDGE ( 'NONE', *, *, #6072, .F. ) ;
#14613 = CARTESIAN_POINT ( 'NONE',  ( -1.399999999999998579, -9.792893218813446765, 3.300000000000000266 ) ) ;
#14614 = VERTEX_POINT ( 'NONE', #15258 ) ;
#14615 = DIRECTION ( 'NONE',  ( 1.000000000000000000, 0.000000000000000000, 6.344131569286600069E-16 ) ) ;
#14616 = CARTESIAN_POINT ( 'NONE',  ( -0.5500000000000000444, -2.399999999999999911, 3.600000000000000089 ) ) ;
#14617 = VERTEX_POINT ( 'NONE', #15540 ) ;
#14618 = VECTOR ( 'NONE', #3806, 1000.000000000000114 ) ;
#14619 = CARTESIAN_POINT ( 'NONE',  ( -0.5999999999999999778, 10.80000000000000071, 7.599999999999999645 ) ) ;
#14620 = CARTESIAN_POINT ( 'NONE',  ( -0.2023972492402590084, -2.146007489747939978, 2.355265251465770149 ) ) ;
#14621 = ADVANCED_FACE ( 'NONE', ( #4308 ), #1087, .F. ) ;
#14622 = LINE ( 'NONE', #1937, #2551 ) ;
#14623 = CARTESIAN_POINT ( 'NONE',  ( -1.003115764947269950, -1.493935417675869903, 6.828967930617589666 ) ) ;
#14624 = CARTESIAN_POINT ( 'NONE',  ( 0.1768565782245979934, -3.752899381639830168, 2.353200596935780098 ) ) ;
#14625 = CARTESIAN_POINT ( 'NONE',  ( -1.872456193198849705, -4.501965483225034426, 5.541908336566010007 ) ) ;
#14626 = LINE ( 'NONE', #7779, #5258 ) ;
#14627 = CARTESIAN_POINT ( 'NONE',  ( -0.5500000000000000444, -2.399999999999999911, 3.600000000000000089 ) ) ;
#14628 = ORIENTED_EDGE ( 'NONE', *, *, #1811, .F. ) ;
#14629 = CARTESIAN_POINT ( 'NONE',  ( 1.965557623688110933, -0.08898305084745804228, 5.292675575926325315 ) ) ;
#14630 = CARTESIAN_POINT ( 'NONE',  ( -2.334032080503389839, -3.310421904162350160, 5.001728246382240783 ) ) ;
#14631 = ORIENTED_EDGE ( 'NONE', *, *, #3431, .T. ) ;
#14632 = EDGE_LOOP ( 'NONE', ( #1078, #15180, #12724, #10638 ) ) ;
#14633 = DIRECTION ( 'NONE',  ( -0.7071067811865500152, 0.000000000000000000, -0.7071067811865451302 ) ) ;
#14634 = VERTEX_POINT ( 'NONE', #15175 ) ;
#14635 = CARTESIAN_POINT ( 'NONE',  ( -0.6673090596498668647, -3.360839357098899693, 2.443133963569591671 ) ) ;
#14636 = VECTOR ( 'NONE', #11813, 1000.000000000000114 ) ;
#14637 = SHAPE_DEFINITION_REPRESENTATION ( #9802, #853 ) ;
#14638 = CARTESIAN_POINT ( 'NONE',  ( -0.9002849211310044453, -5.166525423728809407, 7.196465912290821443 ) ) ;
#14639 = DIRECTION ( 'NONE',  ( 1.608122649676639805E-16, 1.000000000000000000, 0.000000000000000000 ) ) ;
#14640 = DIRECTION ( 'NONE',  ( 2.220446049250309876E-16, 1.000000000000000000, -2.385026923874314915E-32 ) ) ;
#14641 = ORIENTED_EDGE ( 'NONE', *, *, #14277, .T. ) ;
#14642 = DIRECTION ( 'NONE',  ( -1.000000000000000000, 0.000000000000000000, 3.965082230804129973E-17 ) ) ;
#14643 = CARTESIAN_POINT ( 'NONE',  ( 1.550000000000000044, -5.599999999999999645, 5.100000000000000533 ) ) ;
#14644 = CARTESIAN_POINT ( 'NONE',  ( 0.8893259633308030487, -3.846052534792983923, 2.849594321892129134 ) ) ;
#14645 = EDGE_CURVE ( 'NONE', #2413, #2147, #12563, .T. ) ;
#14646 = CARTESIAN_POINT ( 'NONE',  ( -2.586172839791708533, -0.5358050847457624943, 4.104546363490954697 ) ) ;
#14647 = ORIENTED_EDGE ( 'NONE', *, *, #9248, .T. ) ;
#14648 = ORIENTED_EDGE ( 'NONE', *, *, #14564, .F. ) ;
#14649 = CARTESIAN_POINT ( 'NONE',  ( -2.353194804772640314, -5.524364406779660008, 4.731327187377240229 ) ) ;
#14650 = APPLICATION_CONTEXT ( 'automotive_design' ) ;
#14652 = VECTOR ( 'NONE', #10001, 1000.000000000000000 ) ;
#14651 =( NAMED_UNIT ( * ) SI_UNIT ( $, .STERADIAN. ) SOLID_ANGLE_UNIT ( ) );
#14653 = EDGE_CURVE ( 'NONE', #7292, #268, #8129, .T. ) ;
#14654 = FACE_OUTER_BOUND ( 'NONE', #15144, .T. ) ;
#14655 = EDGE_CURVE ( 'NONE', #8501, #16536, #4035, .T. ) ;
#14656 = CARTESIAN_POINT ( 'NONE',  ( 0.2041457401074358857, -4.498124606865046893, 7.346023093209487875 ) ) ;
#14657 = ORIENTED_EDGE ( 'NONE', *, *, #6663, .T. ) ;
#14658 = CARTESIAN_POINT ( 'NONE',  ( -2.352760675243210198, -3.034803321062869763, 4.757121734156080528 ) ) ;
#14659 = LINE ( 'NONE', #600, #4908 ) ;
#14660 = DIRECTION ( 'NONE',  ( 2.220446049250309876E-16, 1.000000000000000000, 0.000000000000000000 ) ) ;
#14661 = CARTESIAN_POINT ( 'NONE',  ( 1.842787987253230897, -3.710163681423226389, 3.794994874786191907 ) ) ;
#14662 = DIRECTION ( 'NONE',  ( -1.000000000000000000, -1.233581138472399909E-16, -2.220446049250309876E-16 ) ) ;
#14663 = VECTOR ( 'NONE', #15971, 1000.000000000000000 ) ;
#14664 = CARTESIAN_POINT ( 'NONE',  ( -1.912899118714301183, -1.381334852594401363, 5.445465495009755408 ) ) ;
#14665 = VERTEX_POINT ( 'NONE', #5353 ) ;
#14666 = ADVANCED_FACE ( 'NONE', ( #16820 ), #18092, .T. ) ;
#14667 = CARTESIAN_POINT ( 'NONE',  ( 1.882879255550339082, -0.4963798976394455664, 2.835213315261639000 ) ) ;
#14668 = ORIENTED_EDGE ( 'NONE', *, *, #8922, .F. ) ;
#14669 = CARTESIAN_POINT ( 'NONE',  ( -1.914021115237000137, -4.754295778036220277, 6.069404563272239983 ) ) ;
#14670 = LINE ( 'NONE', #1989, #6302 ) ;
#14671 = VECTOR ( 'NONE', #4899, 1000.000000000000000 ) ;
#14672 = CARTESIAN_POINT ( 'NONE',  ( 0.1749999999999999889, 9.199999999999999289, 0.4000000000000000222 ) ) ;
#14673 = CARTESIAN_POINT ( 'NONE',  ( -2.270487904532170198, -5.237711864406779938, 4.080813552109679776 ) ) ;
#14674 = ORIENTED_EDGE ( 'NONE', *, *, #1088, .F. ) ;
#14675 = EDGE_CURVE ( 'NONE', #4371, #2194, #7115, .T. ) ;
#14676 = EDGE_LOOP ( 'NONE', ( #3719, #1617, #62, #2977 ) ) ;
#14677 = DIRECTION ( 'NONE',  ( 0.000000000000000000, 0.000000000000000000, 1.000000000000000000 ) ) ;
#14678 = ADVANCED_FACE ( 'NONE', ( #12388 ), #5527, .F. ) ;
#14679 = DIRECTION ( 'NONE',  ( 1.000000000000000000, 0.000000000000000000, 0.000000000000000000 ) ) ;
#14680 = CARTESIAN_POINT ( 'NONE',  ( 0.5637478356992829953, -0.6606104644819250638, 2.398845082743519708 ) ) ;
#14681 = ORIENTED_EDGE ( 'NONE', *, *, #17766, .F. ) ;
#14682 = CIRCLE ( 'NONE', #218, 0.09999999999999982514 ) ;
#14683 = B_SPLINE_CURVE_WITH_KNOTS ( 'NONE', 3,
 ( #3628, #7802, #6597, #5118, #13269, #4828, #9278, #10575, #10478, #16229, #14939, #3536, #12067, #7899, #17687, #10678, #866, #16876, #16608, #5313, #18137, #13999, #9563, #4184, #3996, #15497, #12524, #9843, #1144, #5399, #8366, #6964, #13918, #8277, #3908, #35, #4095, #2806, #15222, #1052, #9750, #1234, #6877, #15135, #2447, #13821, #2527, #8176, #15416, #8093, #2721, #13733, #6688, #9650, #1317, #10864, #12346, #17968, #10960, #11127, #16512, #14084 ),
 .UNSPECIFIED., .F., .F.,
 ( 4, 1, 1, 1, 1, 1, 1, 1, 1, 1, 1, 1, 1, 1, 1, 1, 1, 1, 1, 1, 1, 1, 1, 1, 1, 1, 1, 1, 1, 1, 1, 1, 1, 1, 1, 1, 1, 1, 1, 1, 1, 1, 1, 1, 1, 1, 1, 1, 1, 1, 1, 1, 1, 1, 1, 1, 1, 1, 1, 4 ),
 ( 0.000000000000000000, 0.09318283294546000906, 0.1863656658909200181, 0.2795484988363799994, 0.3727313317818400362, 0.4659141647272999620, 0.5590969976727599988, 0.6522798306182200356, 0.7454626635636800724, 0.8386454965091399982, 0.9318283294545990358, 1.025011162400059961, 1.118193995345519998, 1.211376828290979812, 1.304559661236440071, 1.397742494181900108, 1.490925327127360145, 1.584108160072819960, 1.677290993018279996, 1.770473825963740033, 1.863656658909199848, 1.956839491854659885, 2.050022324800119922, 2.143205157745580181, 2.236387990691039995, 2.329570823636499810, 2.422753656581960069, 2.515936489527420328, 2.609119322472880143, 2.702302155418339957, 2.795484988363799772, 2.888667821309260031, 2.981850654254720290, 3.075033487200179660, 3.168216320145639919, 3.261399153091099734, 3.354581986036559993, 3.447764818982019808, 3.540947651927480067, 3.634130484872939437, 3.727313317818399696, 3.820496150763859955, 3.913678983709319770, 4.006861816654780029, 4.100044649600239843, 4.193227482545699658, 4.286410315491160361, 4.379593148436620176, 4.472775981382079991, 4.565958814327539805, 4.659141647272999620, 4.752324480218450553, 4.845507313163910368, 4.938690146109370183, 5.031872979054829997, 5.125055812000289812, 5.218238644945749627, 5.311421477891210330, 5.404604310836670145, 5.497787143782139729 ),
 .UNSPECIFIED. ) ;
#14684 = VECTOR ( 'NONE', #10161, 1000.000000000000000 ) ;
#14685 = VECTOR ( 'NONE', #14968, 1000.000000000000000 ) ;
#14686 = CARTESIAN_POINT ( 'NONE',  ( -0.6015868932279860859, -3.007674156414608557, 7.284803068494427158 ) ) ;
#14687 = CARTESIAN_POINT ( 'NONE',  ( 1.250000000000000000, 6.144112549695419645, 6.100000000000000533 ) ) ;
#14688 = FACE_OUTER_BOUND ( 'NONE', #10797, .T. ) ;
#14689 = VECTOR ( 'NONE', #3426, 1000.000000000000000 ) ;
#14690 = CARTESIAN_POINT ( 'NONE',  ( -2.226511124464849889, -4.525253771513310319, 5.462491901673850236 ) ) ;
#14691 = CIRCLE ( 'NONE', #8188, 0.2500000000000002220 ) ;
#14692 = CARTESIAN_POINT ( 'NONE',  ( 0.8534102632286154622, -5.320452325212860600, 2.829778315381550780 ) ) ;
#14693 = CARTESIAN_POINT ( 'NONE',  ( -1.820241257191459905, -5.080331814072259533, 3.208199930689799917 ) ) ;
#14694 = AXIS2_PLACEMENT_3D ( 'NONE', #10069, #15722, #4410 ) ;
#14695 = AXIS2_PLACEMENT_3D ( 'NONE', #15089, #2484, #1460 ) ;
#14696 = LINE ( 'NONE', #3492, #2781 ) ;
#14697 = CARTESIAN_POINT ( 'NONE',  ( -1.661700935788390288, -0.2625000000000000111, 3.038299064211610112 ) ) ;
#14698 = CARTESIAN_POINT ( 'NONE',  ( 2.508228811380011081, -5.390889830508485581, 5.566973598334535644 ) ) ;
#14699 = ORIENTED_EDGE ( 'NONE', *, *, #12223, .F. ) ;
#14700 = EDGE_CURVE ( 'NONE', #8906, #17990, #16645, .T. ) ;
#14701 = LINE ( 'NONE', #13227, #135 ) ;
#14702 = ORIENTED_EDGE ( 'NONE', *, *, #15495, .F. ) ;
#14703 = DIRECTION ( 'NONE',  ( 0.000000000000000000, -0.7492686492653550800, 0.6622661785325220096 ) ) ;
#14704 = DIRECTION ( 'NONE',  ( 0.000000000000000000, 1.000000000000000000, 0.000000000000000000 ) ) ;
#14705 = VECTOR ( 'NONE', #9555, 1000.000000000000000 ) ;
#14706 = VECTOR ( 'NONE', #4269, 1000.000000000000000 ) ;
#14707 = ORIENTED_EDGE ( 'NONE', *, *, #3751, .F. ) ;
#14708 = CARTESIAN_POINT ( 'NONE',  ( -0.09706517602693919000, -2.961097579838030125, 7.051451474958980725 ) ) ;
#14709 = FACE_OUTER_BOUND ( 'NONE', #15800, .T. ) ;
#14710 = CARTESIAN_POINT ( 'NONE',  ( 2.500000000000000000, 2.000000000000000000, 1.600000000000000089 ) ) ;
#14711 = DIRECTION ( 'NONE',  ( 3.172065784643310388E-16, 1.000000000000000000, -1.586032892321649771E-16 ) ) ;
#14712 = EDGE_CURVE ( 'NONE', #9165, #9351, #1118, .T. ) ;
#14713 = CARTESIAN_POINT ( 'NONE',  ( 0.4985810152601650724, -1.330917399657850053, 7.000035360316460675 ) ) ;
#14714 = CARTESIAN_POINT ( 'NONE',  ( -0.8934014991059870958, -4.614566048306490309, 6.877287176483410924 ) ) ;
#14715 = VECTOR ( 'NONE', #8845, 1000.000000000000000 ) ;
#14716 = CARTESIAN_POINT ( 'NONE',  ( -2.050563521385710075, -4.595118636378185073, 4.800454404529219232 ) ) ;
#14717 = AXIS2_PLACEMENT_3D ( 'NONE', #4505, #8418, #5812 ) ;
#14718 = FACE_OUTER_BOUND ( 'NONE', #1456, .T. ) ;
#14719 = FACE_OUTER_BOUND ( 'NONE', #13344, .T. ) ;
#14720 = AXIS2_PLACEMENT_3D ( 'NONE', #3407, #11492, #15844 ) ;
#14721 = ORIENTED_EDGE ( 'NONE', *, *, #8733, .F. ) ;
#14722 = DIRECTION ( 'NONE',  ( 0.000000000000000000, -1.000000000000000000, 0.000000000000000000 ) ) ;
#14723 = EDGE_CURVE ( 'NONE', #4957, #138, #11080, .T. ) ;
#14724 = AXIS2_PLACEMENT_3D ( 'NONE', #16813, #15252, #15166 ) ;
#14725 = CARTESIAN_POINT ( 'NONE',  ( -2.034805890357269220, -0.2313559322033900412, 4.427518626519226785 ) ) ;
#14726 = CARTESIAN_POINT ( 'NONE',  ( -0.04278372834682089842, -3.729611093351540063, 2.346934926511239805 ) ) ;
#14727 = VERTEX_POINT ( 'NONE', #1272 ) ;
#14728 = EDGE_LOOP ( 'NONE', ( #393, #14681, #5667, #7898 ) ) ;
#14729 = CARTESIAN_POINT ( 'NONE',  ( -6.735557395310447447E-17, 7.250000000000000000, 6.299999999999997158 ) ) ;
#14730 = VERTEX_POINT ( 'NONE', #16722 ) ;
#14731 = DIRECTION ( 'NONE',  ( 1.306144734853129823E-16, -1.000000000000000000, -6.530723674265629391E-17 ) ) ;
#14732 = AXIS2_PLACEMENT_3D ( 'NONE', #7825, #3460, #9109 ) ;
#14733 = CONTEXT_DEPENDENT_SHAPE_REPRESENTATION ( #13470, #6360 ) ;
#14734 = CARTESIAN_POINT ( 'NONE',  ( -1.800129581279449775, -5.264406779661021218, 2.750028594811118943 ) ) ;
#14735 = VECTOR ( 'NONE', #12404, 1000.000000000000000 ) ;
#14736 = CARTESIAN_POINT ( 'NONE',  ( -1.750000000000000000, 11.40000000000000036, 7.550000000000000711 ) ) ;
#14737 = CARTESIAN_POINT ( 'NONE',  ( 2.500000000000000000, 2.000000000000000000, 1.600000000000000089 ) ) ;
#14738 = VERTEX_POINT ( 'NONE', #14039 ) ;
#14739 = AXIS2_PLACEMENT_3D ( 'NONE', #7257, #11684, #10298 ) ;
#14740 = CARTESIAN_POINT ( 'NONE',  ( 0.1749999999999999889, 9.099999999999999645, 0.5999999999999999778 ) ) ;
#14741 = CARTESIAN_POINT ( 'NONE',  ( 0.5500000000000000444, 6.450000000000000178, 2.699264068711930253 ) ) ;
#14742 = CARTESIAN_POINT ( 'NONE',  ( 1.800000000000000044, 0.5999999999999999778, 6.599999999999999645 ) ) ;
#14743 = CARTESIAN_POINT ( 'NONE',  ( -1.777111910197670008, -3.473439922180372452, 3.672004328189223621 ) ) ;
#14744 = CARTESIAN_POINT ( 'NONE',  ( 2.087380238839969593, -0.1067796610169500227, 6.338810156469096846 ) ) ;
#14745 = ORIENTED_EDGE ( 'NONE', *, *, #2128, .F. ) ;
#14746 = CARTESIAN_POINT ( 'NONE',  ( 1.248294325655350034, -0.3266949152542379942, 2.704938983774300088 ) ) ;
#14747 = VECTOR ( 'NONE', #17604, 1000.000000000000000 ) ;
#14748 = CARTESIAN_POINT ( 'NONE',  ( -2.625437065641401446, -0.5180084745762725262, 5.087214675345155257 ) ) ;
#14749 = ORIENTED_EDGE ( 'NONE', *, *, #9107, .T. ) ;
#14750 = CARTESIAN_POINT ( 'NONE',  ( -1.428515267734880023, -5.568855932203390147, 2.829745655876930055 ) ) ;
#14751 = CARTESIAN_POINT ( 'NONE',  ( 2.352190863465239978, -0.6826862039457533005, 4.622903765856330338 ) ) ;
#14752 = CARTESIAN_POINT ( 'NONE',  ( -0.009452110982655715157, -0.5998079552954631577, 2.050000000000001155 ) ) ;
#14753 = ADVANCED_FACE ( 'NONE', ( #12754 ), #4220, .F. ) ;
#14754 = CARTESIAN_POINT ( 'NONE',  ( -2.652303127816829864, -3.333710192450643373, 4.791661394135809715 ) ) ;
#14755 = ORIENTED_EDGE ( 'NONE', *, *, #14655, .T. ) ;
#14756 = EDGE_CURVE ( 'NONE', #13339, #18164, #5626, .T. ) ;
#14757 = VECTOR ( 'NONE', #5744, 1000.000000000000000 ) ;
#14758 = CARTESIAN_POINT ( 'NONE',  ( -0.8748826269293140667, -3.337551068810609589, 2.515205712983220376 ) ) ;
#14759 = CARTESIAN_POINT ( 'NONE',  ( 1.899999999999999911, 0.4000000000000000222, -2.399999999999999911 ) ) ;
#14760 = PLANE ( 'NONE',  #17007 ) ;
#14761 = CARTESIAN_POINT ( 'NONE',  ( -0.9361665894546699063, -3.314262780522333696, 2.872845392579789880 ) ) ;
#14762 = CARTESIAN_POINT ( 'NONE',  ( -0.5500000000000000444, 6.450000000000000178, 2.699264068711930253 ) ) ;
#14763 = DIRECTION ( 'NONE',  ( -4.379659758543260954E-15, 1.000000000000000000, 0.000000000000000000 ) ) ;
#14764 = CARTESIAN_POINT ( 'NONE',  ( -1.632144308286139989, -1.311469987729540376, 5.945394234592896510 ) ) ;
#14765 = ORIENTED_EDGE ( 'NONE', *, *, #11938, .F. ) ;
#14766 = DIRECTION ( 'NONE',  ( 2.986159789035700404E-15, -1.110223024625159992E-16, -1.000000000000000000 ) ) ;
#14767 = CARTESIAN_POINT ( 'NONE',  ( 1.526064881623949931, -0.7763906680874419486, 2.903976516638540062 ) ) ;
#14768 = CARTESIAN_POINT ( 'NONE',  ( 1.008962495263989956, -0.9854339516935015642, 7.154609617872576877 ) ) ;
#14769 = EDGE_LOOP ( 'NONE', ( #13878, #10680, #5451, #5751 ) ) ;
#14770 = AXIS2_PLACEMENT_3D ( 'NONE', #284, #5923, #13139 ) ;
#14771 = DIRECTION ( 'NONE',  ( 2.035408878479449976E-15, -1.000000000000000000, -9.251858538542959255E-17 ) ) ;
#14772 = CARTESIAN_POINT ( 'NONE',  ( 2.500000000000000000, 0.8000000000000000444, -2.399999999999999911 ) ) ;
#14773 = CARTESIAN_POINT ( 'NONE',  ( -1.750000000000000000, 11.40000000000000036, 7.599999999999999645 ) ) ;
#14774 = CARTESIAN_POINT ( 'NONE',  ( 1.449568901432419343, -5.037500000000000533, 3.250431098567584165 ) ) ;
#14775 = VERTEX_POINT ( 'NONE', #9880 ) ;
#14776 = VERTEX_POINT ( 'NONE', #2840 ) ;
#14777 = CARTESIAN_POINT ( 'NONE',  ( 2.500000000000000000, 4.700000000000000178, 1.600000000000000089 ) ) ;
#14778 = LINE ( 'NONE', #7941, #9999 ) ;
#14779 = CARTESIAN_POINT ( 'NONE',  ( -2.500000000000000000, 11.29999999999999893, 1.600000000000000089 ) ) ;
#14780 = ORIENTED_EDGE ( 'NONE', *, *, #2868, .T. ) ;
#14781 = CARTESIAN_POINT ( 'NONE',  ( 0.9490039995898825742, -3.523857375116919322, 2.221592224478729172 ) ) ;
#14782 = FACE_OUTER_BOUND ( 'NONE', #9967, .T. ) ;
#14783 = CARTESIAN_POINT ( 'NONE',  ( -0.3578984759183553854, -2.984385868126320673, 7.329643012642057087 ) ) ;
#14784 = ADVANCED_FACE ( 'NONE', ( #69 ), #5715, .F. ) ;
#14785 = DIRECTION ( 'NONE',  ( 0.000000000000000000, -1.000000000000000000, -5.224578939412490694E-16 ) ) ;
#14786 = CARTESIAN_POINT ( 'NONE',  ( 0.3367924244280819934, 2.254758922476410188, 7.700000000000000178 ) ) ;
#14787 = VECTOR ( 'NONE', #14591, 1000.000000000000000 ) ;
#14788 = CARTESIAN_POINT ( 'NONE',  ( 1.236334101859160040, -3.570433951693499974, 2.697445712080689617 ) ) ;
#14789 = EDGE_CURVE ( 'NONE', #12528, #17729, #10222, .T. ) ;
#14790 = CARTESIAN_POINT ( 'NONE',  ( -0.5999999999999999778, 7.347880794884128857E-17, 7.700000000000000178 ) ) ;
#14791 = CARTESIAN_POINT ( 'NONE',  ( 1.875000000000000000, 11.25000000000000000, 7.700000000000000178 ) ) ;
#14793 = VERTEX_POINT ( 'NONE', #17247 ) ;
#14792 = CARTESIAN_POINT ( 'NONE',  ( 2.339254516529669647, -2.681638120378568857, 5.953396186326336270 ) ) ;
#14794 = EDGE_CURVE ( 'NONE', #851, #8308, #13018, .T. ) ;
#14795 = DIRECTION ( 'NONE',  ( -1.000000000000000000, 0.000000000000000000, 0.000000000000000000 ) ) ;
#14796 = ADVANCED_FACE ( 'NONE', ( #1730 ), #8933, .T. ) ;
#14797 = CYLINDRICAL_SURFACE ( 'NONE', #18263, 0.3999999999999999667 ) ;
#14798 =( BOUNDED_SURFACE ( )  B_SPLINE_SURFACE ( 3, 3, ( 
 ( #14034, #15353, #12652, #13758, #2657, #5620, #11264, #16548, #3856, #9875, #15534, #8122, #1080, #6725, #16638, #5346, #3939, #146, #15629, #1544, #9964, #11355, #4302, #7193, #2937, #8578, #14226, #12832, #16989, #3780, #3591, #723, #5078, #6648, #9327, #10438, #2211, #6272, #6358, #6465, #922, #12216, #13410, #631, #13609, #6561, #14996, #4879, #9439, #12302, #17832, #9143, #16465, #5166, #12128, #7673, #3498, #12023, #4983, #15102, #2412, #13506 ),
 ( #17925, #9236, #11931, #16100, #17644, #2114, #10637, #3396, #8059, #16190, #10729, #14804, #9040, #14698, #16375, #13701, #1012, #7765, #13314, #14899, #7855, #3961, #9611, #18103, #6747, #12399, #8500, #18018, #5637, #5365, #9890, #11006, #6841, #15273, #15549, #15371, #1098, #13877, #2577, #10923, #11280, #4142, #16732, #2853, #1192, #4230, #12485, #5450, #15186, #2494, #5539, #5270, #11090, #16832, #12766, #4049, #9704, #8143, #9800, #14150, #16568, #4411 ),
 ( #2674, #3875, #1471, #15460, #8326, #7131, #13962, #13777, #1282, #6925, #12572, #2768, #18185, #8413, #14048, #1364, #7025, #12672, #14592, #7291, #4684, #2956, #15903, #12848, #4319, #7391, #12937, #10154, #15649, #266, #11457, #10233, #1908, #16001, #3212, #4498, #5990, #8862, #7555, #162, #8596, #1741, #79, #5904, #4576, #15730, #5724, #14244, #14510, #1561, #3036, #8675, #14416, #14324, #11722, #11545, #1644, #13028, #11370, #11630, #17003, #15808 ),
 ( #9984, #3304, #7206, #1831, #7474, #17178, #17092, #10078, #5808, #351, #13122, #434, #3114, #4419, #6074, #17355, #8766, #8947, #17807, #521, #13295, #17721, #2388, #13201, #5053, #16350, #13478, #3467, #3563, #11827, #6170, #14874, #1992, #17450, #4768, #16164, #4858, #614, #6432, #10420, #12101, #16081, #3378, #6335, #3654, #9022, #14673, #7739, #10705, #9304, #16260, #10608, #6252, #7650, #15077, #11999, #11910, #17530, #9117, #10504, #13385, #9411 ),
 ( #14774, #2088, #14971, #699, #2283, #17616, #4954, #9210, #7936, #2188, #7831, #794, #13584, #899, #6535, #12191, #5144, #10795, #16441, #3749, #10896, #12554, #8394, #15531, #2749, #15349, #14031, #1172, #4122, #986, #8034, #6906, #1345, #8206, #12646, #11261, #18271, #6722, #5617, #13944, #11067, #13674, #6622, #16711, #9871, #16903, #18083, #2553, #2654, #4024, #5241, #4210, #13853, #12280, #12375, #9678, #1261, #6998, #8307, #17901, #1077, #16545 ),
 ( #16809, #18163, #16635, #3853, #9781, #15442, #9506, #17997, #15161, #3935, #2472, #5343, #10987, #8118, #6820, #5514, #11160, #13755, #9589, #15249, #12465, #5430, #11527, #7457, #6053, #8479, #144, #12746, #414, #9961, #7371, #11610, #5791, #14224, #12830, #4661, #10134, #5968, #4558, #1628, #15625, #17239, #3192, #2933, #14121, #15880, #1542, #8844, #14491, #4478, #61, #7190, #11435, #15710, #333, #1815, #5884, #243, #17072, #10318, #2832, #14308 ),
 ( #1447, #15791, #8574, #7107, #5707, #4399, #10054, #3017, #14392, #11352, #13011, #16985, #4299, #12916, #13098, #8658, #17157, #3099, #8744, #11700, #17332, #17512, #16234, #5121, #3439, #4836, #495, #2165, #16326, #15979, #10682, #4922, #3631, #9088, #12072, #14572, #3285, #14851, #9282, #16138, #2253, #870, #7905, #14649, #13556, #9188, #674, #1886, #7533, #6314, #17785, #6509, #7719, #14750, #10579, #11977, #13177, #12168, #2063, #6145, #1966, #17588 ) ),
 .UNSPECIFIED., .T., .F., .F. ) 
 B_SPLINE_SURFACE_WITH_KNOTS ( ( 4, 3, 4 ),
 ( 4, 1, 1, 1, 1, 1, 1, 1, 1, 1, 1, 1, 1, 1, 1, 1, 1, 1, 1, 1, 1, 1, 1, 1, 1, 1, 1, 1, 1, 1, 1, 1, 1, 1, 1, 1, 1, 1, 1, 1, 1, 1, 1, 1, 1, 1, 1, 1, 1, 1, 1, 1, 1, 1, 1, 1, 1, 1, 1, 4 ),
 ( 0.000000000000000000, 3.141592653589790007, 6.283185307179590673 ),
 ( 0.7853981633974479459, 0.8785809963429079827, 0.9717638292883680196, 1.064946662233830166, 1.158129495179289981, 1.251312328124750017, 1.344495161070210054, 1.437677994015669869, 1.530860826961130128, 1.624043659906589943, 1.717226492852049979, 1.810409325797510016, 1.903592158742969831, 1.996774991688430090, 2.089957824633889683, 2.183140657579349941, 2.276323490524809756, 2.369506323470270015, 2.462689156415730274, 2.555871989361190089, 2.649054822306649903, 2.742237655252109718, 2.835420488197569977, 2.928603321143030236, 3.021786154088490051, 3.114968987033949865, 3.208151819979410124, 3.301334652924869939, 3.394517485870330198, 3.487700318815790013, 3.580883151761249827, 3.674065984706710086, 3.767248817652169901, 3.860431650597620390, 3.953614483543080205, 4.046797316488540019, 4.139980149433999834, 4.233162982379460537, 4.326345815324920352, 4.419528648270380167, 4.512711481215839981, 4.605894314161299796, 4.699077147106759611, 4.792259980052219426, 4.885442812997680129, 4.978625645943139943, 5.071808478888599758, 5.164991311834059573, 5.258174144779520276, 5.351356977724980091, 5.444539810670439905, 5.537722643615899720, 5.630905476561360423, 5.724088309506820238, 5.817271142452280053, 5.910453975397739868, 6.003636808343199682, 6.096819641288659497, 6.190002474234119312, 6.283185307179590673 ),
 .UNSPECIFIED. ) 
 GEOMETRIC_REPRESENTATION_ITEM ( )  RATIONAL_B_SPLINE_SURFACE ( (
 ( 1.000000000000000000, 1.000000000000000000, 1.000000000000000000, 1.000000000000000000, 1.000000000000000000, 1.000000000000000000, 1.000000000000000000, 1.000000000000000000, 1.000000000000000000, 1.000000000000000000, 1.000000000000000000, 1.000000000000000000, 1.000000000000000000, 1.000000000000000000, 1.000000000000000000, 1.000000000000000000, 1.000000000000000000, 1.000000000000000000, 1.000000000000000000, 1.000000000000000000, 1.000000000000000000, 1.000000000000000000, 1.000000000000000000, 1.000000000000000000, 1.000000000000000000, 1.000000000000000000, 1.000000000000000000, 1.000000000000000000, 1.000000000000000000, 1.000000000000000000, 1.000000000000000000, 1.000000000000000000, 1.000000000000000000, 1.000000000000000000, 1.000000000000000000, 1.000000000000000000, 1.000000000000000000, 1.000000000000000000, 1.000000000000000000, 1.000000000000000000, 1.000000000000000000, 1.000000000000000000, 1.000000000000000000, 1.000000000000000000, 1.000000000000000000, 1.000000000000000000, 1.000000000000000000, 1.000000000000000000, 1.000000000000000000, 1.000000000000000000, 1.000000000000000000, 1.000000000000000000, 1.000000000000000000, 1.000000000000000000, 1.000000000000000000, 1.000000000000000000, 1.000000000000000000, 1.000000000000000000, 1.000000000000000000, 1.000000000000000000, 1.000000000000000000, 1.000000000000000000),
 ( 0.3333333333333329818, 0.3333333333333329818, 0.3333333333333329818, 0.3333333333333329818, 0.3333333333333329818, 0.3333333333333329818, 0.3333333333333329818, 0.3333333333333329818, 0.3333333333333329818, 0.3333333333333329818, 0.3333333333333329818, 0.3333333333333329818, 0.3333333333333329818, 0.3333333333333329818, 0.3333333333333329818, 0.3333333333333329818, 0.3333333333333329818, 0.3333333333333329818, 0.3333333333333329818, 0.3333333333333329818, 0.3333333333333329818, 0.3333333333333329818, 0.3333333333333329818, 0.3333333333333329818, 0.3333333333333329818, 0.3333333333333329818, 0.3333333333333329818, 0.3333333333333329818, 0.3333333333333329818, 0.3333333333333329818, 0.3333333333333329818, 0.3333333333333329818, 0.3333333333333329818, 0.3333333333333329818, 0.3333333333333329818, 0.3333333333333329818, 0.3333333333333329818, 0.3333333333333329818, 0.3333333333333329818, 0.3333333333333329818, 0.3333333333333329818, 0.3333333333333329818, 0.3333333333333329818, 0.3333333333333329818, 0.3333333333333329818, 0.3333333333333329818, 0.3333333333333329818, 0.3333333333333329818, 0.3333333333333329818, 0.3333333333333329818, 0.3333333333333329818, 0.3333333333333329818, 0.3333333333333329818, 0.3333333333333329818, 0.3333333333333329818, 0.3333333333333329818, 0.3333333333333329818, 0.3333333333333329818, 0.3333333333333329818, 0.3333333333333329818, 0.3333333333333329818, 0.3333333333333329818),
 ( 0.3333333333333329818, 0.3333333333333329818, 0.3333333333333329818, 0.3333333333333329818, 0.3333333333333329818, 0.3333333333333329818, 0.3333333333333329818, 0.3333333333333329818, 0.3333333333333329818, 0.3333333333333329818, 0.3333333333333329818, 0.3333333333333329818, 0.3333333333333329818, 0.3333333333333329818, 0.3333333333333329818, 0.3333333333333329818, 0.3333333333333329818, 0.3333333333333329818, 0.3333333333333329818, 0.3333333333333329818, 0.3333333333333329818, 0.3333333333333329818, 0.3333333333333329818, 0.3333333333333329818, 0.3333333333333329818, 0.3333333333333329818, 0.3333333333333329818, 0.3333333333333329818, 0.3333333333333329818, 0.3333333333333329818, 0.3333333333333329818, 0.3333333333333329818, 0.3333333333333329818, 0.3333333333333329818, 0.3333333333333329818, 0.3333333333333329818, 0.3333333333333329818, 0.3333333333333329818, 0.3333333333333329818, 0.3333333333333329818, 0.3333333333333329818, 0.3333333333333329818, 0.3333333333333329818, 0.3333333333333329818, 0.3333333333333329818, 0.3333333333333329818, 0.3333333333333329818, 0.3333333333333329818, 0.3333333333333329818, 0.3333333333333329818, 0.3333333333333329818, 0.3333333333333329818, 0.3333333333333329818, 0.3333333333333329818, 0.3333333333333329818, 0.3333333333333329818, 0.3333333333333329818, 0.3333333333333329818, 0.3333333333333329818, 0.3333333333333329818, 0.3333333333333329818, 0.3333333333333329818),
 ( 1.000000000000000000, 1.000000000000000000, 1.000000000000000000, 1.000000000000000000, 1.000000000000000000, 1.000000000000000000, 1.000000000000000000, 1.000000000000000000, 1.000000000000000000, 1.000000000000000000, 1.000000000000000000, 1.000000000000000000, 1.000000000000000000, 1.000000000000000000, 1.000000000000000000, 1.000000000000000000, 1.000000000000000000, 1.000000000000000000, 1.000000000000000000, 1.000000000000000000, 1.000000000000000000, 1.000000000000000000, 1.000000000000000000, 1.000000000000000000, 1.000000000000000000, 1.000000000000000000, 1.000000000000000000, 1.000000000000000000, 1.000000000000000000, 1.000000000000000000, 1.000000000000000000, 1.000000000000000000, 1.000000000000000000, 1.000000000000000000, 1.000000000000000000, 1.000000000000000000, 1.000000000000000000, 1.000000000000000000, 1.000000000000000000, 1.000000000000000000, 1.000000000000000000, 1.000000000000000000, 1.000000000000000000, 1.000000000000000000, 1.000000000000000000, 1.000000000000000000, 1.000000000000000000, 1.000000000000000000, 1.000000000000000000, 1.000000000000000000, 1.000000000000000000, 1.000000000000000000, 1.000000000000000000, 1.000000000000000000, 1.000000000000000000, 1.000000000000000000, 1.000000000000000000, 1.000000000000000000, 1.000000000000000000, 1.000000000000000000, 1.000000000000000000, 1.000000000000000000),
 ( 0.3333333333333329818, 0.3333333333333329818, 0.3333333333333329818, 0.3333333333333329818, 0.3333333333333329818, 0.3333333333333329818, 0.3333333333333329818, 0.3333333333333329818, 0.3333333333333329818, 0.3333333333333329818, 0.3333333333333329818, 0.3333333333333329818, 0.3333333333333329818, 0.3333333333333329818, 0.3333333333333329818, 0.3333333333333329818, 0.3333333333333329818, 0.3333333333333329818, 0.3333333333333329818, 0.3333333333333329818, 0.3333333333333329818, 0.3333333333333329818, 0.3333333333333329818, 0.3333333333333329818, 0.3333333333333329818, 0.3333333333333329818, 0.3333333333333329818, 0.3333333333333329818, 0.3333333333333329818, 0.3333333333333329818, 0.3333333333333329818, 0.3333333333333329818, 0.3333333333333329818, 0.3333333333333329818, 0.3333333333333329818, 0.3333333333333329818, 0.3333333333333329818, 0.3333333333333329818, 0.3333333333333329818, 0.3333333333333329818, 0.3333333333333329818, 0.3333333333333329818, 0.3333333333333329818, 0.3333333333333329818, 0.3333333333333329818, 0.3333333333333329818, 0.3333333333333329818, 0.3333333333333329818, 0.3333333333333329818, 0.3333333333333329818, 0.3333333333333329818, 0.3333333333333329818, 0.3333333333333329818, 0.3333333333333329818, 0.3333333333333329818, 0.3333333333333329818, 0.3333333333333329818, 0.3333333333333329818, 0.3333333333333329818, 0.3333333333333329818, 0.3333333333333329818, 0.3333333333333329818),
 ( 0.3333333333333329818, 0.3333333333333329818, 0.3333333333333329818, 0.3333333333333329818, 0.3333333333333329818, 0.3333333333333329818, 0.3333333333333329818, 0.3333333333333329818, 0.3333333333333329818, 0.3333333333333329818, 0.3333333333333329818, 0.3333333333333329818, 0.3333333333333329818, 0.3333333333333329818, 0.3333333333333329818, 0.3333333333333329818, 0.3333333333333329818, 0.3333333333333329818, 0.3333333333333329818, 0.3333333333333329818, 0.3333333333333329818, 0.3333333333333329818, 0.3333333333333329818, 0.3333333333333329818, 0.3333333333333329818, 0.3333333333333329818, 0.3333333333333329818, 0.3333333333333329818, 0.3333333333333329818, 0.3333333333333329818, 0.3333333333333329818, 0.3333333333333329818, 0.3333333333333329818, 0.3333333333333329818, 0.3333333333333329818, 0.3333333333333329818, 0.3333333333333329818, 0.3333333333333329818, 0.3333333333333329818, 0.3333333333333329818, 0.3333333333333329818, 0.3333333333333329818, 0.3333333333333329818, 0.3333333333333329818, 0.3333333333333329818, 0.3333333333333329818, 0.3333333333333329818, 0.3333333333333329818, 0.3333333333333329818, 0.3333333333333329818, 0.3333333333333329818, 0.3333333333333329818, 0.3333333333333329818, 0.3333333333333329818, 0.3333333333333329818, 0.3333333333333329818, 0.3333333333333329818, 0.3333333333333329818, 0.3333333333333329818, 0.3333333333333329818, 0.3333333333333329818, 0.3333333333333329818),
 ( 1.000000000000000000, 1.000000000000000000, 1.000000000000000000, 1.000000000000000000, 1.000000000000000000, 1.000000000000000000, 1.000000000000000000, 1.000000000000000000, 1.000000000000000000, 1.000000000000000000, 1.000000000000000000, 1.000000000000000000, 1.000000000000000000, 1.000000000000000000, 1.000000000000000000, 1.000000000000000000, 1.000000000000000000, 1.000000000000000000, 1.000000000000000000, 1.000000000000000000, 1.000000000000000000, 1.000000000000000000, 1.000000000000000000, 1.000000000000000000, 1.000000000000000000, 1.000000000000000000, 1.000000000000000000, 1.000000000000000000, 1.000000000000000000, 1.000000000000000000, 1.000000000000000000, 1.000000000000000000, 1.000000000000000000, 1.000000000000000000, 1.000000000000000000, 1.000000000000000000, 1.000000000000000000, 1.000000000000000000, 1.000000000000000000, 1.000000000000000000, 1.000000000000000000, 1.000000000000000000, 1.000000000000000000, 1.000000000000000000, 1.000000000000000000, 1.000000000000000000, 1.000000000000000000, 1.000000000000000000, 1.000000000000000000, 1.000000000000000000, 1.000000000000000000, 1.000000000000000000, 1.000000000000000000, 1.000000000000000000, 1.000000000000000000, 1.000000000000000000, 1.000000000000000000, 1.000000000000000000, 1.000000000000000000, 1.000000000000000000, 1.000000000000000000, 1.000000000000000000) ) ) 
 REPRESENTATION_ITEM ( '' )  SURFACE ( )  );
#14799 = PLANE ( 'NONE',  #2319 ) ;
#14800 = CARTESIAN_POINT ( 'NONE',  ( -1.850000000000000089, 0.7500000000000000000, 8.300000000000000711 ) ) ;
#14801 = CARTESIAN_POINT ( 'NONE',  ( 1.644832646965660006, -1.191187669928119863, 6.383232381746459794 ) ) ;
#14802 = CARTESIAN_POINT ( 'NONE',  ( 1.378221871957440170, -0.4201271186440679872, 6.607619368096269596 ) ) ;
#14803 = DIRECTION ( 'NONE',  ( 1.000000000000000000, 0.000000000000000000, 0.000000000000000000 ) ) ;
#14804 = CARTESIAN_POINT ( 'NONE',  ( 2.625437065641401446, -5.381991525423726053, 5.087214675345139270 ) ) ;
#14805 = ORIENTED_EDGE ( 'NONE', *, *, #7682, .T. ) ;
#14806 = PLANE ( 'NONE',  #3674 ) ;
#14807 = VERTEX_POINT ( 'NONE', #4408 ) ;
#14808 = CARTESIAN_POINT ( 'NONE',  ( -0.1749999999999999889, 9.299999999999998934, 0.5999999999999999778 ) ) ;
#14809 = CIRCLE ( 'NONE', #11270, 0.5999999999999998668 ) ;
#14810 = LINE ( 'NONE', #14616, #14157 ) ;
#14811 = ORIENTED_EDGE ( 'NONE', *, *, #16562, .T. ) ;
#14812 = ORIENTED_EDGE ( 'NONE', *, *, #7123, .T. ) ;
#14813 = CARTESIAN_POINT ( 'NONE',  ( -1.881914957835490121, -1.936412895153350133, 3.286797332666350435 ) ) ;
#14814 = DIRECTION ( 'NONE',  ( 0.000000000000000000, 0.4472135954999599261, -0.8944271909999148562 ) ) ;
#14815 = CYLINDRICAL_SURFACE ( 'NONE', #5543, 0.5000000000000004441 ) ;
#14816 = DIRECTION ( 'NONE',  ( -1.000000000000000000, 0.000000000000000000, 0.000000000000000000 ) ) ;
#14817 = EDGE_CURVE ( 'NONE', #14474, #4438, #11812, .T. ) ;
#14818 = CARTESIAN_POINT ( 'NONE',  ( -2.316639661709700260, -1.819971453711900056, 4.285359956977770501 ) ) ;
#14819 = CARTESIAN_POINT ( 'NONE',  ( -1.097561405233230092, -3.613169651910099756, 2.618148744692269769 ) ) ;
#14820 = CARTESIAN_POINT ( 'NONE',  ( 1.658519201881180738, -2.402178660919109365, 3.489952108543023623 ) ) ;
#14821 = CARTESIAN_POINT ( 'NONE',  ( 0.6964468257805941365, -0.1334745762711869732, 6.631228347243847132 ) ) ;
#14822 = CARTESIAN_POINT ( 'NONE',  ( 0.1749999999999999889, 7.900000000000000355, 0.4000000000000000222 ) ) ;
#14823 = CARTESIAN_POINT ( 'NONE',  ( 1.438959988998139914E-16, -0.2999999999999999889, 2.350000000000000089 ) ) ;
#14824 = LINE ( 'NONE', #2137, #2658 ) ;
#14825 = ORIENTED_EDGE ( 'NONE', *, *, #13107, .F. ) ;
#14826 = CARTESIAN_POINT ( 'NONE',  ( 1.564316099353070033, -5.123660385842499387, 3.135683900646930145 ) ) ;
#14827 = LINE ( 'NONE', #2140, #13166 ) ;
#14828 = CARTESIAN_POINT ( 'NONE',  ( -2.295719155670160383, -3.287133615874060055, 5.218091927917240191 ) ) ;
#14829 = VERTEX_POINT ( 'NONE', #4487 ) ;
#14830 = ORIENTED_EDGE ( 'NONE', *, *, #4348, .T. ) ;
#14831 = PLANE ( 'NONE',  #8242 ) ;
#14832 = VERTEX_POINT ( 'NONE', #11535 ) ;
#14833 = CARTESIAN_POINT ( 'NONE',  ( -0.7500000000000000000, 6.450000000000000178, 2.699264068711930253 ) ) ;
#14834 = PRODUCT_CONTEXT ( 'NONE', #830, 'mechanical' ) ;
#14835 = CARTESIAN_POINT ( 'NONE',  ( -2.203023580853999963, -5.242161016949149932, 3.872235369154300333 ) ) ;
#14836 = CARTESIAN_POINT ( 'NONE',  ( 1.800000000000000044, 0.5999999999999999778, 7.599999999999999645 ) ) ;
#14837 = CARTESIAN_POINT ( 'NONE',  ( 2.500000000000000000, 9.199999999999999289, 1.600000000000000089 ) ) ;
#14838 = CARTESIAN_POINT ( 'NONE',  ( -1.811729841638700211, -0.5580508474576270084, 3.197954009834299782 ) ) ;
#14839 = VERTEX_POINT ( 'NONE', #17079 ) ;
#14840 = EDGE_CURVE ( 'NONE', #8832, #9239, #10326, .T. ) ;
#14841 = LINE ( 'NONE', #1956, #3155 ) ;
#14842 = DIRECTION ( 'NONE',  ( 0.000000000000000000, 6.123233995736769734E-17, -1.000000000000000000 ) ) ;
#14843 = CARTESIAN_POINT ( 'NONE',  ( 1.508881462028659692, -4.311818300558746486, 6.092184821126257255 ) ) ;
#14844 = CARTESIAN_POINT ( 'NONE',  ( 0.9002849211310119948, -0.1334745762711869732, 7.196465912290821443 ) ) ;
#14845 = VERTEX_POINT ( 'NONE', #14402 ) ;
#14846 = CARTESIAN_POINT ( 'NONE',  ( 1.750316316486830059, -0.3400423728813560253, 3.126818518378580158 ) ) ;
#14847 = VERTEX_POINT ( 'NONE', #7541 ) ;
#14848 = CARTESIAN_POINT ( 'NONE',  ( -1.254903241568450900, -0.4735169491525429986, 7.038391080368498365 ) ) ;
#14849 = VERTEX_POINT ( 'NONE', #12838 ) ;
#14850 = LINE ( 'NONE', #17873, #16290 ) ;
#14851 = CARTESIAN_POINT ( 'NONE',  ( -1.978267656359410154, -5.497669491525420504, 5.974740860598790171 ) ) ;
#14852 = CARTESIAN_POINT ( 'NONE',  ( 0.2335786437626899970, 6.450000000000000178, 2.241421356237310203 ) ) ;
#14853 = CARTESIAN_POINT ( 'NONE',  ( 2.159308672244681482, -0.8457042219637719294, 6.242886823772496818 ) ) ;
#14854 = ORIENTED_EDGE ( 'NONE', *, *, #5373, .F. ) ;
#14855 = CARTESIAN_POINT ( 'NONE',  ( -0.3865907654992132292, -4.952022267818764867, 2.675656795012148592 ) ) ;
#14856 = CIRCLE ( 'NONE', #667, 0.01000000000000002623 ) ;
#14857 = CARTESIAN_POINT ( 'NONE',  ( -0.1226612266410539998, -2.662190708450249854, 7.050255286338659388 ) ) ;
#14858 = EDGE_CURVE ( 'NONE', #14730, #13146, #15797, .T. ) ;
#14859 = LINE ( 'NONE', #8018, #10226 ) ;
#14860 = CARTESIAN_POINT ( 'NONE',  ( -2.616666666666669805, -4.318079751576579732E-16, 4.000000000000000000 ) ) ;
#14861 = CARTESIAN_POINT ( 'NONE',  ( -0.2475374578675481607, -4.245794312053864594, 6.738044908627027318 ) ) ;
#14862 = FACE_BOUND ( 'NONE', #1700, .T. ) ;
#14863 = LINE ( 'NONE', #13374, #14747 ) ;
#14864 = CARTESIAN_POINT ( 'NONE',  ( -1.831349212334698828, -1.590929447188999646, 3.772065786216939554 ) ) ;
#14865 = ORIENTED_EDGE ( 'NONE', *, *, #18093, .T. ) ;
#14866 = LINE ( 'NONE', #12370, #4078 ) ;
#14867 = CARTESIAN_POINT ( 'NONE',  ( 1.495970331552388455, -0.4480353997208171291, 2.495424373718078570 ) ) ;
#14868 = CARTESIAN_POINT ( 'NONE',  ( 1.700860513939579599, -2.475884402143949892, 6.737200825918507441 ) ) ;
#14869 = CIRCLE ( 'NONE', #4223, 0.5999999999999998668 ) ;
#14870 = ORIENTED_EDGE ( 'NONE', *, *, #2975, .T. ) ;
#14871 = DIRECTION ( 'NONE',  ( 2.220446049250309876E-16, 0.000000000000000000, -1.000000000000000000 ) ) ;
#14872 = CARTESIAN_POINT ( 'NONE',  ( -4.898587196589400133E-17, 5.318248954186070243, 6.599999999999999645 ) ) ;
#14873 = CARTESIAN_POINT ( 'NONE',  ( -1.875000000000000000, 0.7500000000000000000, 7.700000000000000178 ) ) ;
#14874 = CARTESIAN_POINT ( 'NONE',  ( -1.000896394980330006, -5.170974576271190948, 6.829956240957379521 ) ) ;
#14875 = ORIENTED_EDGE ( 'NONE', *, *, #639, .T. ) ;
#14876 = ORIENTED_EDGE ( 'NONE', *, *, #15750, .F. ) ;
#14877 = PLANE ( 'NONE',  #926 ) ;
#14878 = LINE ( 'NONE', #4862, #16497 ) ;
#14879 = FACE_OUTER_BOUND ( 'NONE', #3710, .T. ) ;
#14880 = ORIENTED_EDGE ( 'NONE', *, *, #16707, .F. ) ;
#14881 = CARTESIAN_POINT ( 'NONE',  ( 2.050059171113549183, -5.377542372881360500, 4.809263467226075228 ) ) ;
#14882 = CARTESIAN_POINT ( 'NONE',  ( -0.5134687485629449988, -3.384127645387192018, 2.096259702418250104 ) ) ;
#14883 = LINE ( 'NONE', #2197, #13873 ) ;
#14884 = CARTESIAN_POINT ( 'NONE',  ( 0.1366863161731129428, -2.937809291549738688, 7.350364228549148393 ) ) ;
#14885 = PLANE ( 'NONE',  #9691 ) ;
#14886 = AXIS2_PLACEMENT_3D ( 'NONE', #11278, #15458, #8594 ) ;
#14887 = DIRECTION ( 'NONE',  ( 3.018987445473099952E-48, 1.000000000000000000, 2.465190328815659976E-32 ) ) ;
#14888 = CARTESIAN_POINT ( 'NONE',  ( 2.111627294540149968, -3.710163681423230386, 3.660877362176659933 ) ) ;
#14889 = FACE_OUTER_BOUND ( 'NONE', #4143, .T. ) ;
#14890 = LINE ( 'NONE', #12119, #6478 ) ;
#14892 = ORIENTED_EDGE ( 'NONE', *, *, #2975, .F. ) ;
#14891 = CARTESIAN_POINT ( 'NONE',  ( -1.292937800126279679, -3.077539021279473097, 7.017633607369056392 ) ) ;
#14893 = CARTESIAN_POINT ( 'NONE',  ( 1.149999999999999911, 9.299999999999998934, 7.500000000000000000 ) ) ;
#14894 = DIRECTION ( 'NONE',  ( 0.000000000000000000, -1.000000000000000000, -8.881784197001250351E-16 ) ) ;
#14895 = PLANE ( 'NONE',  #10434 ) ;
#14896 = CARTESIAN_POINT ( 'NONE',  ( 0.8748826269292639957, -2.262448931189380286, 2.515205712983200392 ) ) ;
#14897 = CARTESIAN_POINT ( 'NONE',  ( -1.925796468768790071, -0.4957627118644070130, 6.052706598917719560 ) ) ;
#14898 = CARTESIAN_POINT ( 'NONE',  ( -1.000000000000000000, -6.000000000000000000, 5.100000000000000533 ) ) ;
#14899 = CARTESIAN_POINT ( 'NONE',  ( 1.666450993087180477, -5.417584745762705545, 6.765380371283858274 ) ) ;
#14900 = VERTEX_POINT ( 'NONE', #9972 ) ;
#14901 = DIRECTION ( 'NONE',  ( 0.000000000000000000, 0.000000000000000000, 1.000000000000000000 ) ) ;
#14902 = ORIENTED_EDGE ( 'NONE', *, *, #1573, .T. ) ;
#14903 = CARTESIAN_POINT ( 'NONE',  ( 2.043308330018789309, -5.099788135593219529, 5.867646457774661428 ) ) ;
#14904 = CARTESIAN_POINT ( 'NONE',  ( -1.250000000000000000, 3.881370849898470254, 6.100000000000000533 ) ) ;
#14905 = LINE ( 'NONE', #13231, #14439 ) ;
#14906 = EDGE_CURVE ( 'NONE', #12720, #13022, #14498, .T. ) ;
#14907 = ORIENTED_EDGE ( 'NONE', *, *, #14270, .F. ) ;
#14908 = EDGE_CURVE ( 'NONE', #6669, #16962, #17640, .T. ) ;
#14909 = EDGE_LOOP ( 'NONE', ( #16041, #944, #12145, #16810 ) ) ;
#14910 = CARTESIAN_POINT ( 'NONE',  ( 0.8748826269292639957, -2.262448931189380286, 2.515205712983200392 ) ) ;
#14911 = CARTESIAN_POINT ( 'NONE',  ( -1.000896394980330006, -5.470974576271190770, 6.829956240957379521 ) ) ;
#14912 = DIRECTION ( 'NONE',  ( 0.000000000000000000, 0.000000000000000000, -1.000000000000000000 ) ) ;
#14913 = CARTESIAN_POINT ( 'NONE',  ( 0.01716182025089369942, -2.169295778036230082, 2.346608583467340026 ) ) ;
#14914 = CARTESIAN_POINT ( 'NONE',  ( -1.460675875430050175, -4.684430913171359734, 6.545310725710059785 ) ) ;
#14915 = CARTESIAN_POINT ( 'NONE',  ( 2.007801995112640903, -2.611773255513701653, 5.128524201241654978 ) ) ;
#14916 = DIRECTION ( 'NONE',  ( -0.7049180327868858065, 1.565232460946939801E-16, -0.7092887755011121342 ) ) ;
#14917 = DIRECTION ( 'NONE',  ( 0.000000000000000000, 0.000000000000000000, -1.000000000000000000 ) ) ;
#14918 = ORIENTED_EDGE ( 'NONE', *, *, #5298, .T. ) ;
#14919 = CARTESIAN_POINT ( 'NONE',  ( 1.618511124886439889, -5.326166231000110329, 3.081488875113560066 ) ) ;
#14920 = EDGE_CURVE ( 'NONE', #17492, #12197, #15637, .T. ) ;
#14921 = CARTESIAN_POINT ( 'NONE',  ( -0.5372984490435469551, 4.599999999999999645, 7.700000000000000178 ) ) ;
#14922 = CARTESIAN_POINT ( 'NONE',  ( -2.159566522375440112, -3.240557039297490061, 5.635424033751089468 ) ) ;
#14923 = VECTOR ( 'NONE', #8061, 1000.000000000000000 ) ;
#14924 = ORIENTED_EDGE ( 'NONE', *, *, #17391, .F. ) ;
#14925 = EDGE_LOOP ( 'NONE', ( #5743, #3138, #15691, #3982 ) ) ;
#14926 = CARTESIAN_POINT ( 'NONE',  ( 0.5291502622129179434, -1.642400929185890127E-16, 7.700000000000000178 ) ) ;
#14927 = ADVANCED_FACE ( 'NONE', ( #341 ), #8757, .T. ) ;
#14928 = VERTEX_POINT ( 'NONE', #14314 ) ;
#14929 = CARTESIAN_POINT ( 'NONE',  ( -2.291237445532080308, -4.664983501243040287, 4.162434510291850742 ) ) ;
#14930 = EDGE_CURVE ( 'NONE', #1590, #16145, #7197, .T. ) ;
#14931 = CARTESIAN_POINT ( 'NONE',  ( 2.293398556041700065, -5.064194915254240037, 4.171956209133470317 ) ) ;
#14932 = ADVANCED_FACE ( 'NONE', ( #8852 ), #5977, .T. ) ;
#14933 = FACE_OUTER_BOUND ( 'NONE', #1145, .T. ) ;
#14934 = CARTESIAN_POINT ( 'NONE',  ( -1.994983296312370147, -1.334758276017820045, 5.948514050749340143 ) ) ;
#14935 = DIRECTION ( 'NONE',  ( -1.000000000000000000, 0.000000000000000000, 1.586032892321649771E-16 ) ) ;
#14936 = CARTESIAN_POINT ( 'NONE',  ( 1.971820545011360171, -4.055647129387581984, 4.128313389260194199 ) ) ;
#14937 = CARTESIAN_POINT ( 'NONE',  ( 0.2189795514005130062, -0.004449152542373159894, 2.356806637999009801 ) ) ;
#14938 = ORIENTED_EDGE ( 'NONE', *, *, #8937, .T. ) ;
#14939 = CARTESIAN_POINT ( 'NONE',  ( 1.750316316486830059, -0.3400423728813560253, 3.126818518378580158 ) ) ;
#14940 = CARTESIAN_POINT ( 'NONE',  ( 2.354888465609351389, -0.09788135593220394226, 5.923664702843856489 ) ) ;
#14941 = ORIENTED_EDGE ( 'NONE', *, *, #17749, .T. ) ;
#14942 = CARTESIAN_POINT ( 'NONE',  ( -0.1749999999999999889, 9.500000000000000000, 1.600000000000000089 ) ) ;
#14943 = CARTESIAN_POINT ( 'NONE',  ( -0.7999999999998790301, 11.40000000000000036, -9.797174393178840942E-17 ) ) ;
#14944 = EDGE_CURVE ( 'NONE', #9567, #16962, #5892, .T. ) ;
#14945 = CARTESIAN_POINT ( 'NONE',  ( 2.218077401483169453, -0.7758393570989060573, 5.486688202856499608 ) ) ;
#14946 = CARTESIAN_POINT ( 'NONE',  ( 1.943632316591230147, -5.346398305084740343, 3.373048379518159834 ) ) ;
#14947 = VECTOR ( 'NONE', #2364, 1000.000000000000000 ) ;
#14948 = CARTESIAN_POINT ( 'NONE',  ( 2.408279507600870950, -0.7991276453871939411, 5.815035204050346351 ) ) ;
#14949 = ORIENTED_EDGE ( 'NONE', *, *, #15508, .T. ) ;
#14950 = DIRECTION ( 'NONE',  ( 2.775557561562890365E-16, 1.000000000000000000, -2.775557561562890365E-16 ) ) ;
#14951 = CARTESIAN_POINT ( 'NONE',  ( 1.934380261529039080, -0.7758393570989061683, 5.387804366397126010 ) ) ;
#14952 = CARTESIAN_POINT ( 'NONE',  ( -1.648422021521479763, -4.684430913171365063, 6.779860219333237126 ) ) ;
#14953 = CARTESIAN_POINT ( 'NONE',  ( -1.850000000000000089, 0.7500000000000000000, 7.700000000000000178 ) ) ;
#14954 = PLANE ( 'NONE',  #13795 ) ;
#14955 = CARTESIAN_POINT ( 'NONE',  ( -0.9742769543504515850, -4.338947465207014353, 6.507120986223577042 ) ) ;
#14956 = PRODUCT_DEFINITION_SHAPE ( 'NONE', 'NONE',  #18297 ) ;
#14957 = PLANE ( 'NONE',  #6122 ) ;
#14958 = FACE_OUTER_BOUND ( 'NONE', #8599, .T. ) ;
#14959 = EDGE_CURVE ( 'NONE', #9457, #5374, #11444, .T. ) ;
#14960 = CARTESIAN_POINT ( 'NONE',  ( 1.777111910197639810, -2.126560077819629413, 3.672004328189181432 ) ) ;
#14961 = VERTEX_POINT ( 'NONE', #6058 ) ;
#14962 = PLANE ( 'NONE',  #5099 ) ;
#14963 = CARTESIAN_POINT ( 'NONE',  ( 0.3750000000000000000, 3.050000000000000266, 2.100000000000000089 ) ) ;
#14964 = AXIS2_PLACEMENT_3D ( 'NONE', #113, #18131, #4357 ) ;
#14965 = CARTESIAN_POINT ( 'NONE',  ( 0.009452110982655428928, -0.3001920447045380858, 2.649999999999998579 ) ) ;
#14966 = CARTESIAN_POINT ( 'NONE',  ( -0.9250303514741213817, -1.777235753495299608, 2.212544966868041474 ) ) ;
#14967 = VERTEX_POINT ( 'NONE', #11707 ) ;
#14968 = DIRECTION ( 'NONE',  ( 6.344131569286609929E-16, 1.000000000000000000, 1.586032892321649771E-16 ) ) ;
#14969 = CARTESIAN_POINT ( 'NONE',  ( 1.850000000000000089, 0.7500000000000000000, 7.649999999999999467 ) ) ;
#14970 = CARTESIAN_POINT ( 'NONE',  ( 2.500000000000000000, 2.000000000000000000, 0.5999999999999999778 ) ) ;
#14971 = CARTESIAN_POINT ( 'NONE',  ( 1.580445181003960586, -5.041949152542365198, 3.389704561770334301 ) ) ;
#14972 = VERTEX_POINT ( 'NONE', #4671 ) ;
#14973 = ADVANCED_FACE ( 'NONE', ( #17517 ), #2263, .T. ) ;
#14974 = ORIENTED_EDGE ( 'NONE', *, *, #4647, .T. ) ;
#14975 = DIRECTION ( 'NONE',  ( 0.000000000000000000, 1.000000000000000000, -1.850371707708589879E-16 ) ) ;
#14976 = FACE_OUTER_BOUND ( 'NONE', #12233, .T. ) ;
#14977 = PLANE ( 'NONE',  #3430 ) ;
#14978 = ORIENTED_EDGE ( 'NONE', *, *, #4732, .T. ) ;
#14979 = VECTOR ( 'NONE', #12604, 1000.000000000000000 ) ;
#14980 = CARTESIAN_POINT ( 'NONE',  ( 2.351526912647309953, -5.373093220338979847, 4.606040641882800379 ) ) ;
#14981 = CARTESIAN_POINT ( 'NONE',  ( 2.632194480419669080, -2.289578095837640159, 5.038623552414890128 ) ) ;
#14982 = CARTESIAN_POINT ( 'NONE',  ( -0.7999999999998730349, 12.00000000000000000, -9.797174393178840942E-17 ) ) ;
#14983 = AXIS2_PLACEMENT_3D ( 'NONE', #2507, #8154, #18035 ) ;
#14984 = VECTOR ( 'NONE', #8382, 1000.000000000000000 ) ;
#14985 = FACE_OUTER_BOUND ( 'NONE', #13140, .T. ) ;
#14986 = CARTESIAN_POINT ( 'NONE',  ( 0.5500000000000000444, -2.399999999999999911, 3.299999999999999822 ) ) ;
#14987 = CARTESIAN_POINT ( 'NONE',  ( 2.199335452462550133, -3.733451969711520491, 3.862342996790889771 ) ) ;
#14988 = DIRECTION ( 'NONE',  ( 2.220446049250309876E-16, 0.000000000000000000, 1.000000000000000000 ) ) ;
#14989 = DIRECTION ( 'NONE',  ( 0.000000000000000000, 1.000000000000000000, 0.000000000000000000 ) ) ;
#14991 = ORIENTED_EDGE ( 'NONE', *, *, #12425, .T. ) ;
#14990 = CARTESIAN_POINT ( 'NONE',  ( 1.094547058713730037, -2.844656138396588929, 7.117660114503893354 ) ) ;
#14992 = CARTESIAN_POINT ( 'NONE',  ( 0.6500000000000000222, 3.050000000000000266, 3.200000000000000178 ) ) ;
#14993 = CARTESIAN_POINT ( 'NONE',  ( 1.115198193348289957, -1.261052534792989954, 6.772457159276550342 ) ) ;
#14994 = DIRECTION ( 'NONE',  ( -1.850371707708589879E-16, -1.000000000000000000, -1.268826313857319964E-16 ) ) ;
#14995 = CYLINDRICAL_SURFACE ( 'NONE', #2056, 0.5000000000000004441 ) ;
#14996 = CARTESIAN_POINT ( 'NONE',  ( -2.270487904532170198, -5.537711864406779760, 4.080813552109679776 ) ) ;
#14997 = ORIENTED_EDGE ( 'NONE', *, *, #1806, .T. ) ;
#14998 = VECTOR ( 'NONE', #12862, 1000.000000000000000 ) ;
#14999 = CARTESIAN_POINT ( 'NONE',  ( 1.477796163681079689, -5.117584745762709275, 6.531563725478138238 ) ) ;
#15000 = DIRECTION ( 'NONE',  ( 2.865091676452019757E-16, 0.000000000000000000, -1.000000000000000000 ) ) ;
#15001 = CARTESIAN_POINT ( 'NONE',  ( 0.009037091307168881177, -0.3067697551340939910, 2.399753621991609798 ) ) ;
#15002 = VECTOR ( 'NONE', #7580, 1000.000000000000000 ) ;
#15003 = ORIENTED_EDGE ( 'NONE', *, *, #11069, .T. ) ;
#15004 = VECTOR ( 'NONE', #10200, 1000.000000000000000 ) ;
#15005 = AXIS2_PLACEMENT_3D ( 'NONE', #4863, #6079, #17264 ) ;
#15006 = CARTESIAN_POINT ( 'NONE',  ( 1.866416942370620058, -3.962493976234419790, 3.266391446483460026 ) ) ;
#15007 = CARTESIAN_POINT ( 'NONE',  ( -2.345900685764729765, -5.528813559322030002, 4.512231114381339836 ) ) ;
#15008 = CARTESIAN_POINT ( 'NONE',  ( 2.500000000000000000, 10.00000000000000000, -1.206091987257470116E-15 ) ) ;
#15009 = AXIS2_PLACEMENT_3D ( 'NONE', #12089, #10694, #16337 ) ;
#15010 = CARTESIAN_POINT ( 'NONE',  ( 0.9719602541832789155, -2.844656138396589817, 6.843370931913530519 ) ) ;
#15011 = VECTOR ( 'NONE', #12408, 1000.000000000000000 ) ;
#15012 = CARTESIAN_POINT ( 'NONE',  ( -2.052909741356249373, -1.773394877135329839, 4.721527574705180363 ) ) ;
#15013 = DIRECTION ( 'NONE',  ( -7.656710514656250048E-17, 0.9659258262890690894, 0.2588190451025180749 ) ) ;
#15014 = EDGE_CURVE ( 'NONE', #18253, #14972, #14659, .T. ) ;
#15015 = CIRCLE ( 'NONE', #12643, 0.1500000000000000777 ) ;
#15016 = CARTESIAN_POINT ( 'NONE',  ( -1.685497504775380850, -0.2673043920988010802, 2.637581209070348987 ) ) ;
#15017 = ORIENTED_EDGE ( 'NONE', *, *, #8695, .T. ) ;
#15018 = CARTESIAN_POINT ( 'NONE',  ( 1.579711282809380002, -5.089528081836459883, 3.120288717190609962 ) ) ;
#15019 = AXIS2_PLACEMENT_3D ( 'NONE', #14461, #15685, #4623 ) ;
#15020 = FACE_OUTER_BOUND ( 'NONE', #11458, .T. ) ;
#15021 = CARTESIAN_POINT ( 'NONE',  ( -2.325590009395030133, -4.870737219477670799, 5.061077271074069905 ) ) ;
#15022 = ORIENTED_EDGE ( 'NONE', *, *, #5312, .F. ) ;
#15023 = VERTEX_POINT ( 'NONE', #10781 ) ;
#15024 = DIRECTION ( 'NONE',  ( -1.643460219210440021E-31, -1.000000000000000000, -2.220446049250309876E-16 ) ) ;
#15025 = TOROIDAL_SURFACE ( 'NONE', #4062, 0.2999999999999999889, 0.2500000000000000000 ) ;
#15026 = ORIENTED_EDGE ( 'NONE', *, *, #12870, .T. ) ;
#15027 = CIRCLE ( 'NONE', #15865, 0.04999999999999969746 ) ;
#15028 = CARTESIAN_POINT ( 'NONE',  ( -1.936998685628559258, -4.758136654396199816, 3.363294429306560751 ) ) ;
#15029 = CARTESIAN_POINT ( 'NONE',  ( 1.791574935211219799, -5.108686440677970175, 6.226029630577610163 ) ) ;
#15030 = AXIS2_PLACEMENT_3D ( 'NONE', #5783, #14213, #8383 ) ;
#15031 = FACE_OUTER_BOUND ( 'NONE', #8732, .T. ) ;
#15032 = VECTOR ( 'NONE', #7273, 1000.000000000000000 ) ;
#15033 = VERTEX_POINT ( 'NONE', #5035 ) ;
#15034 = CARTESIAN_POINT ( 'NONE',  ( 1.626408692231650077, -0.8922807985403480302, 6.401040991074950171 ) ) ;
#15035 = AXIS2_PLACEMENT_3D ( 'NONE', #18206, #13798, #12231 ) ;
#15036 = EDGE_CURVE ( 'NONE', #4096, #4195, #16149, .T. ) ;
#15037 = DIRECTION ( 'NONE',  ( -1.000000000000000000, 0.000000000000000000, 8.326672684688679970E-16 ) ) ;
#15038 = CARTESIAN_POINT ( 'NONE',  ( 0.2818998297622880012, -1.354205687946139935, 7.036509827384409554 ) ) ;
#15039 = PRODUCT_DEFINITION ( 'UNKNOWN', '', #7103, #15123 ) ;
#15040 = AXIS2_PLACEMENT_3D ( 'NONE', #3145, #7328, #13062 ) ;
#15041 = EDGE_CURVE ( 'NONE', #1835, #15121, #3449, .T. ) ;
#15042 = CARTESIAN_POINT ( 'NONE',  ( 2.088297318559229954, -0.09788135593220401165, 5.785136623276629919 ) ) ;
#15043 = VECTOR ( 'NONE', #13667, 1000.000000000000000 ) ;
#15044 = VERTEX_POINT ( 'NONE', #14953 ) ;
#15045 = AXIS2_PLACEMENT_3D ( 'NONE', #8116, #9504, #16346 ) ;
#15046 = EDGE_CURVE ( 'NONE', #9755, #10260, #7888, .T. ) ;
#15047 = EDGE_CURVE ( 'NONE', #10006, #4096, #14859, .T. ) ;
#15048 = CARTESIAN_POINT ( 'NONE',  ( 2.203023580853990193, -0.05783898305084790581, 3.872235369154280349 ) ) ;
#15049 = ORIENTED_EDGE ( 'NONE', *, *, #15830, .T. ) ;
#15050 = VECTOR ( 'NONE', #3870, 1000.000000000000000 ) ;
#15051 = AXIS2_PLACEMENT_3D ( 'NONE', #14182, #10174, #9914 ) ;
#15052 = DIRECTION ( 'NONE',  ( 0.000000000000000000, -1.000000000000000000, 0.000000000000000000 ) ) ;
#15053 = CARTESIAN_POINT ( 'NONE',  ( -0.1824815401349519361, -1.101875393134940317, 7.046368721022736814 ) ) ;
#15054 = CARTESIAN_POINT ( 'NONE',  ( -0.8244235255442939891, -0.5829339996946389935, 2.492493020344019872 ) ) ;
#15055 = CARTESIAN_POINT ( 'NONE',  ( 0.04351999560419626129, -1.078587104846650213, 7.353529668759038351 ) ) ;
#15056 = ORIENTED_EDGE ( 'NONE', *, *, #9930, .T. ) ;
#15057 = VECTOR ( 'NONE', #6970, 1000.000000000000000 ) ;
#15058 = FACE_OUTER_BOUND ( 'NONE', #12281, .T. ) ;
#15059 = CARTESIAN_POINT ( 'NONE',  ( 1.552749016687789974, -4.036199717459258984, 6.468535037441730751 ) ) ;
#15060 = CARTESIAN_POINT ( 'NONE',  ( 2.370419177058800120, -4.241953435693877061, 5.893409660608535994 ) ) ;
#15061 = DIRECTION ( 'NONE',  ( -1.000000000000000000, 2.220446049250309876E-16, 6.049014748177260544E-16 ) ) ;
#15062 = FACE_OUTER_BOUND ( 'NONE', #493, .T. ) ;
#15063 = VECTOR ( 'NONE', #10225, 1000.000000000000000 ) ;
#15064 = CARTESIAN_POINT ( 'NONE',  ( -0.2047443300700520219, -3.407415933675483899, 2.657212296411530783 ) ) ;
#15065 = EDGE_CURVE ( 'NONE', #13803, #8938, #6414, .T. ) ;
#15066 = CARTESIAN_POINT ( 'NONE',  ( -1.850000000000000089, 11.25000000000000000, 7.649999999999999467 ) ) ;
#15067 = CARTESIAN_POINT ( 'NONE',  ( -0.1526488871098711508, -1.847100618360169699, 2.652660223633551251 ) ) ;
#15068 = ORIENTED_EDGE ( 'NONE', *, *, #4570, .F. ) ;
#15069 = FACE_OUTER_BOUND ( 'NONE', #4994, .T. ) ;
#15070 = CARTESIAN_POINT ( 'NONE',  ( 1.899999999999999911, 10.00000000000000000, 1.600000000000000089 ) ) ;
#15071 = AXIS2_PLACEMENT_3D ( 'NONE', #5103, #6929, #10754 ) ;
#15072 = CARTESIAN_POINT ( 'NONE',  ( 0.2451610102875899921, -0.3251990024832500104, 2.350791033861340029 ) ) ;
#15073 = CARTESIAN_POINT ( 'NONE',  ( 0.6015868932280445947, -2.592325843585391532, 7.284803068494412948 ) ) ;
#15074 = EDGE_LOOP ( 'NONE', ( #11371, #6969, #9807, #1212 ) ) ;
#15075 = CARTESIAN_POINT ( 'NONE',  ( 0.1749999999999999889, 6.799999999999999822, 1.600000000000000089 ) ) ;
#15076 = CARTESIAN_POINT ( 'NONE',  ( -1.505092429369619955, -5.128627060139309357, 2.879659483602799774 ) ) ;
#15077 = CARTESIAN_POINT ( 'NONE',  ( -1.248294325655370018, -5.273305084745760318, 2.704938983774309857 ) ) ;
#15078 = ORIENTED_EDGE ( 'NONE', *, *, #4710, .T. ) ;
#15079 = VERTEX_POINT ( 'NONE', #17704 ) ;
#15080 = CARTESIAN_POINT ( 'NONE',  ( 1.110223024625159893E-15, 0.3005290370886140594, 5.295654259262600583 ) ) ;
#15081 = DIRECTION ( 'NONE',  ( 2.960594732333750117E-16, -1.000000000000000000, 0.000000000000000000 ) ) ;
#15082 = AXIS2_PLACEMENT_3D ( 'NONE', #7428, #470, #1942 ) ;
#15083 = DIRECTION ( 'NONE',  ( 1.586032892321649771E-16, -1.000000000000000000, -7.930164461608259947E-17 ) ) ;
#15084 = ORIENTED_EDGE ( 'NONE', *, *, #2225, .F. ) ;
#15085 = CARTESIAN_POINT ( 'NONE',  ( 0.06264882350516240428, -5.448728813559320372, 7.052569299041220319 ) ) ;
#15086 = CARTESIAN_POINT ( 'NONE',  ( 1.752195476665078688, -4.036199717459260761, 6.693219682964302031 ) ) ;
#15087 = CARTESIAN_POINT ( 'NONE',  ( 0.2451610102875898256, -0.3251990024832499548, 2.350791033861340029 ) ) ;
#15088 = EDGE_CURVE ( 'NONE', #8344, #14551, #11374, .T. ) ;
#15089 = CARTESIAN_POINT ( 'NONE',  ( -1.899999999999999911, 0.5999999999999999778, 7.599999999999999645 ) ) ;
#15090 = CARTESIAN_POINT ( 'NONE',  ( 1.881914957835459923, -3.663587104846649734, 3.286797332666310023 ) ) ;
#15092 = ADVANCED_FACE ( 'NONE', ( #2071 ), #16243, .T. ) ;
#15091 = CARTESIAN_POINT ( 'NONE',  ( -1.899999999999999911, 9.199999999999999289, 0.6099999999999999867 ) ) ;
#15093 = DIRECTION ( 'NONE',  ( 1.000000000000000000, 0.000000000000000000, 0.000000000000000000 ) ) ;
#15095 = ORIENTED_EDGE ( 'NONE', *, *, #9585, .T. ) ;
#15094 = CARTESIAN_POINT ( 'NONE',  ( 1.524497189778211581, -2.798079561820010941, 6.872331008700157007 ) ) ;
#15096 = VECTOR ( 'NONE', #17112, 1000.000000000000000 ) ;
#15097 = CARTESIAN_POINT ( 'NONE',  ( -0.1749999999999999889, 6.799999999999999822, 0.5999999999999999778 ) ) ;
#15098 = DIRECTION ( 'NONE',  ( 0.000000000000000000, 0.000000000000000000, 1.000000000000000000 ) ) ;
#15099 = CARTESIAN_POINT ( 'NONE',  ( -1.881914957835490121, -1.936412895153350133, 3.286797332666350435 ) ) ;
#15100 = CARTESIAN_POINT ( 'NONE',  ( -0.1749999999999999889, 9.099999999999999645, 0.4000000000000000222 ) ) ;
#15101 = CARTESIAN_POINT ( 'NONE',  ( 0.1749999999999999889, 7.700000000000000178, 0.4000000000000000222 ) ) ;
#15102 = CARTESIAN_POINT ( 'NONE',  ( -0.2189795514005259958, -5.595550847457629651, 2.356806637999020015 ) ) ;
#15103 = VERTEX_POINT ( 'NONE', #11984 ) ;
#15104 = FACE_OUTER_BOUND ( 'NONE', #16600, .T. ) ;
#15105 = CARTESIAN_POINT ( 'NONE',  ( 1.149999999999999911, 6.447051294741199534, 6.942609934460510779 ) ) ;
#15106 = CARTESIAN_POINT ( 'NONE',  ( -0.009340024727881909850, -0.5980314830687609717, 2.378874508206480165 ) ) ;
#15107 = ORIENTED_EDGE ( 'NONE', *, *, #2128, .T. ) ;
#15108 = VECTOR ( 'NONE', #15879, 1000.000000000000000 ) ;
#15109 = CARTESIAN_POINT ( 'NONE',  ( -2.326448859701059746, -3.380286769027220029, 4.344498395672320434 ) ) ;
#15110 = CARTESIAN_POINT ( 'NONE',  ( -1.549742865090599997, -5.484322033898309634, 6.471102547561460305 ) ) ;
#15111 = DIRECTION ( 'NONE',  ( 0.3420201433256691015, 0.000000000000000000, -0.9396926207859082059 ) ) ;
#15112 = DIRECTION ( 'NONE',  ( -1.000000000000000000, 0.000000000000000000, 0.000000000000000000 ) ) ;
#15113 = CARTESIAN_POINT ( 'NONE',  ( 2.126557263589630153, -2.448755237495689574, 3.691783806836010040 ) ) ;
#15114 = CARTESIAN_POINT ( 'NONE',  ( -1.699999999999999956, 9.299999999999998934, 7.599999999999999645 ) ) ;
#15115 = CARTESIAN_POINT ( 'NONE',  ( 0.4365326870214371602, -1.330917399657850497, 6.706076034398976482 ) ) ;
#15116 = DIRECTION ( 'NONE',  ( -1.000000000000000000, 0.000000000000000000, 0.000000000000000000 ) ) ;
#15117 = AXIS2_PLACEMENT_3D ( 'NONE', #3215, #14421, #1834 ) ;
#15118 = DIRECTION ( 'NONE',  ( 0.000000000000000000, 0.000000000000000000, 1.000000000000000000 ) ) ;
#15119 = ORIENTED_EDGE ( 'NONE', *, *, #10853, .F. ) ;
#15120 = DIRECTION ( 'NONE',  ( -1.000000000000000000, 0.000000000000000000, 0.000000000000000000 ) ) ;
#15121 = VERTEX_POINT ( 'NONE', #3639 ) ;
#15122 = ORIENTED_EDGE ( 'NONE', *, *, #14488, .T. ) ;
#15123 = PRODUCT_DEFINITION_CONTEXT ( 'detailed design', #15980, 'design' ) ;
#15124 = ORIENTED_EDGE ( 'NONE', *, *, #18149, .T. ) ;
#15125 = LINE ( 'NONE', #2342, #8027 ) ;
#15126 = CARTESIAN_POINT ( 'NONE',  ( 1.661700935788380074, -5.037500000000000533, 3.038299064211610112 ) ) ;
#15127 = VECTOR ( 'NONE', #5199, 1000.000000000000000 ) ;
#15128 = CYLINDRICAL_SURFACE ( 'NONE', #11139, 0.6000000000000000888 ) ;
#15129 = CARTESIAN_POINT ( 'NONE',  ( 0.9499999999999999556, 2.299999999999999822, 7.599999999999999645 ) ) ;
#15130 = CARTESIAN_POINT ( 'NONE',  ( -2.651429253058529945, -4.618406924666464519, 4.585822029124955179 ) ) ;
#15131 = LINE ( 'NONE', #3992, #2297 ) ;
#15132 = CARTESIAN_POINT ( 'NONE',  ( -1.503462833636818541, -5.095857339597785973, 3.304888304972901647 ) ) ;
#15133 = CARTESIAN_POINT ( 'NONE',  ( 1.057242234132090175, -0.02224576271186469792, 2.597442975781520058 ) ) ;
#15134 = ORIENTED_EDGE ( 'NONE', *, *, #13566, .T. ) ;
#15135 = CARTESIAN_POINT ( 'NONE',  ( -1.641808337277740115, -0.4868644067796619734, 6.386111670537629514 ) ) ;
#15136 = ORIENTED_EDGE ( 'NONE', *, *, #5074, .F. ) ;
#15137 = CARTESIAN_POINT ( 'NONE',  ( -2.586172839791708533, -0.2358050847457631438, 4.104546363490954697 ) ) ;
#15138 = ORIENTED_EDGE ( 'NONE', *, *, #10737, .F. ) ;
#15139 = FACE_OUTER_BOUND ( 'NONE', #4129, .T. ) ;
#15140 = CARTESIAN_POINT ( 'NONE',  ( 1.722199153441389852, -0.5041426604022090086, 3.099360556065540173 ) ) ;
#15141 = CARTESIAN_POINT ( 'NONE',  ( -2.340070819011249803, -5.519915254237290014, 4.950151441910549899 ) ) ;
#15142 = EDGE_CURVE ( 'NONE', #7904, #10219, #10691, .T. ) ;
#15143 = CARTESIAN_POINT ( 'NONE',  ( 2.589817782457058737, -0.6361096273691766445, 4.120381550729950604 ) ) ;
#15144 = EDGE_LOOP ( 'NONE', ( #929, #14069, #4109, #10070 ) ) ;
#15145 = CARTESIAN_POINT ( 'NONE',  ( 0.009452110982653675123, -5.000192044704546035, 2.649999999999998579 ) ) ;
#15146 = ADVANCED_FACE ( 'NONE', ( #12176 ), #2174, .T. ) ;
#15147 = CARTESIAN_POINT ( 'NONE',  ( 1.886482464143609095, -0.5895330507926000996, 3.890008792968652429 ) ) ;
#15148 = ADVANCED_FACE ( 'NONE', ( #4937 ), #13659, .F. ) ;
#15149 = LINE ( 'NONE', #8190, #3424 ) ;
#15150 = LINE ( 'NONE', #12542, #8525 ) ;
#15151 = CARTESIAN_POINT ( 'NONE',  ( 1.942813984510739056, -1.074746228486680000, 5.363608065214415355 ) ) ;
#15152 = PLANE ( 'NONE',  #4653 ) ;
#15153 = ORIENTED_EDGE ( 'NONE', *, *, #14000, .T. ) ;
#15154 = FACE_OUTER_BOUND ( 'NONE', #7987, .T. ) ;
#15155 = FACE_OUTER_BOUND ( 'NONE', #4851, .T. ) ;
#15156 = FACE_OUTER_BOUND ( 'NONE', #7495, .T. ) ;
#15157 = CARTESIAN_POINT ( 'NONE',  ( 0.8400312909773258729, -2.569037555297099651, 7.217431453521787610 ) ) ;
#15158 = EDGE_LOOP ( 'NONE', ( #9590, #8899, #5505, #15331 ) ) ;
#15159 = DIRECTION ( 'NONE',  ( 8.223874256482639351E-17, -1.000000000000000000, 0.000000000000000000 ) ) ;
#15160 = CARTESIAN_POINT ( 'NONE',  ( 2.500000000000000000, 2.000000000000000000, -1.695950706916410117E-15 ) ) ;
#15161 = CARTESIAN_POINT ( 'NONE',  ( 2.034805890357269220, -5.368644067796615182, 4.427518626519221456 ) ) ;
#15162 = EDGE_LOOP ( 'NONE', ( #894, #14674, #5126, #16103 ) ) ;
#15163 = VECTOR ( 'NONE', #10336, 1000.000000000000000 ) ;
#15164 = EDGE_CURVE ( 'NONE', #12277, #16854, #12026, .T. ) ;
#15165 = DIRECTION ( 'NONE',  ( 1.000000000000000000, 0.000000000000000000, 0.000000000000000000 ) ) ;
#15166 = DIRECTION ( 'NONE',  ( 0.000000000000000000, 0.000000000000000000, -1.000000000000000000 ) ) ;
#15167 = DIRECTION ( 'NONE',  ( 0.000000000000000000, 0.000000000000000000, -1.000000000000000000 ) ) ;
#15168 = EDGE_CURVE ( 'NONE', #6864, #14832, #16334, .T. ) ;
#15169 = VERTEX_POINT ( 'NONE', #971 ) ;
#15170 = CARTESIAN_POINT ( 'NONE',  ( -2.203023580853999963, -5.542161016949149754, 3.872235369154300333 ) ) ;
#15171 = EDGE_CURVE ( 'NONE', #4627, #17672, #16426, .T. ) ;
#15172 = CARTESIAN_POINT ( 'NONE',  ( -0.8001094918299070935, -4.292370888630430592, 7.230402832373842514 ) ) ;
#15173 = CARTESIAN_POINT ( 'NONE',  ( 0.9866023595736961305, -5.020626044399128851, 2.560054107758460873 ) ) ;
#15174 = CARTESIAN_POINT ( 'NONE',  ( -0.04661003995944364847, -3.729611093351542284, 2.046522810126899294 ) ) ;
#15175 = CARTESIAN_POINT ( 'NONE',  ( 1.983927814618709873E-15, 10.80000000000000071, 7.500000000000000000 ) ) ;
#15176 = CARTESIAN_POINT ( 'NONE',  ( -1.652654650382400003, -4.804713230972780025, 3.029252778805629820 ) ) ;
#15177 = DIRECTION ( 'NONE',  ( 1.387778780781449866E-16, 1.110223024625160090E-15, 1.000000000000000000 ) ) ;
#15178 = DIRECTION ( 'NONE',  ( 0.000000000000000000, 0.000000000000000000, -1.000000000000000000 ) ) ;
#15179 = AXIS2_PLACEMENT_3D ( 'NONE', #9866, #16705, #1166 ) ;
#15180 = ORIENTED_EDGE ( 'NONE', *, *, #10246, .T. ) ;
#15181 = CARTESIAN_POINT ( 'NONE',  ( -1.850000000000000089, 0.7500000000000000000, 7.649999999999999467 ) ) ;
#15182 = CARTESIAN_POINT ( 'NONE',  ( 2.180207327701309872, -0.3934322033898309812, 5.586116916730190063 ) ) ;
#15183 = CARTESIAN_POINT ( 'NONE',  ( 2.023259452208809872, -2.425466949207399914, 3.497849062500220096 ) ) ;
#15184 = CARTESIAN_POINT ( 'NONE',  ( -0.008236272907986450995, -5.280537951349149495, 2.272810616177459941 ) ) ;
#15185 = LINE ( 'NONE', #3779, #8872 ) ;
#15186 = CARTESIAN_POINT ( 'NONE',  ( -2.386628511786350160, -5.546610169491530407, 3.539457309197792778 ) ) ;
#15187 = ORIENTED_EDGE ( 'NONE', *, *, #17726, .T. ) ;
#15188 = PLANE ( 'NONE',  #1621 ) ;
#15189 = CARTESIAN_POINT ( 'NONE',  ( 2.234315482767909700, -5.059745762711858497, 3.960850823455320580 ) ) ;
#15190 = DIRECTION ( 'NONE',  ( 0.000000000000000000, -1.000000000000000000, 0.000000000000000000 ) ) ;
#15191 = DIRECTION ( 'NONE',  ( -1.608122649676639805E-16, -1.000000000000000000, 0.000000000000000000 ) ) ;
#15192 = EDGE_CURVE ( 'NONE', #2742, #12909, #12265, .T. ) ;
#15193 = ORIENTED_EDGE ( 'NONE', *, *, #7449, .F. ) ;
#15194 = CARTESIAN_POINT ( 'NONE',  ( 0.6096110657044089276, -3.799475958216410376, 2.426869991387509806 ) ) ;
#15195 = CARTESIAN_POINT ( 'NONE',  ( -2.500000000000000000, 8.500000000000000000, 0.6099999999999999867 ) ) ;
#15196 = CARTESIAN_POINT ( 'NONE',  ( -1.750316316486840051, -5.559957627118639500, 3.126818518378589928 ) ) ;
#15197 = DIRECTION ( 'NONE',  ( -1.000000000000000000, 2.220446049250309876E-16, 6.123233995736769734E-17 ) ) ;
#15198 = CARTESIAN_POINT ( 'NONE',  ( 0.8748826269292639957, -2.262448931189380286, 2.515205712983200392 ) ) ;
#15199 = VECTOR ( 'NONE', #6379, 1000.000000000000000 ) ;
#15200 = CARTESIAN_POINT ( 'NONE',  ( -2.352190863465239978, -4.917313796054239461, 4.622903765856379188 ) ) ;
#15201 = CARTESIAN_POINT ( 'NONE',  ( -1.238036348455400670, -2.006277760018210898, 3.062267469172299528 ) ) ;
#15202 = VECTOR ( 'NONE', #5901, 1000.000000000000000 ) ;
#15203 = CARTESIAN_POINT ( 'NONE',  ( 1.899999999999999911, 2.000000000000000000, 0.5999999999999999778 ) ) ;
#15204 = ORIENTED_EDGE ( 'NONE', *, *, #16035, .T. ) ;
#15205 = CARTESIAN_POINT ( 'NONE',  ( 1.399999999999999911, 5.799999999999999822, 7.700000000000000178 ) ) ;
#15206 = CARTESIAN_POINT ( 'NONE',  ( -2.033393610350109793, -4.777584066324510381, 5.884928737465370041 ) ) ;
#15207 = EDGE_CURVE ( 'NONE', #103, #9728, #6892, .T. ) ;
#15208 = ORIENTED_EDGE ( 'NONE', *, *, #9822, .F. ) ;
#15209 = ORIENTED_EDGE ( 'NONE', *, *, #15614, .T. ) ;
#15210 = EDGE_CURVE ( 'NONE', #3744, #8531, #9769, .T. ) ;
#15211 = ORIENTED_EDGE ( 'NONE', *, *, #1873, .F. ) ;
#15212 = PLANE ( 'NONE',  #4100 ) ;
#15213 = CARTESIAN_POINT ( 'NONE',  ( -0.7983658734557950165, -5.166525423728809407, 6.913847129767330735 ) ) ;
#15214 = DIRECTION ( 'NONE',  ( -1.142385477618690076E-14, 1.110223024625153952E-16, -1.000000000000000000 ) ) ;
#15215 = ORIENTED_EDGE ( 'NONE', *, *, #16254, .T. ) ;
#15216 = CARTESIAN_POINT ( 'NONE',  ( -2.584100759211431786, -4.664983501243040287, 4.095403473953163953 ) ) ;
#15217 = EDGE_CURVE ( 'NONE', #18244, #6584, #15336, .T. ) ;
#15218 = DIRECTION ( 'NONE',  ( 4.440892098500630106E-16, 0.000000000000000000, -1.000000000000000000 ) ) ;
#15219 = CARTESIAN_POINT ( 'NONE',  ( 1.480680413335799805, -1.214475958216410190, 6.529298007719799735 ) ) ;
#15220 = CARTESIAN_POINT ( 'NONE',  ( -2.191755591049691532, -0.2536016949152540834, 3.203650300307721466 ) ) ;
#15221 = ORIENTED_EDGE ( 'NONE', *, *, #17323, .T. ) ;
#15222 = CARTESIAN_POINT ( 'NONE',  ( -0.7093417302541390468, -0.4646186440677970153, 6.943956659919700236 ) ) ;
#15223 = ORIENTED_EDGE ( 'NONE', *, *, #3966, .F. ) ;
#15224 = CARTESIAN_POINT ( 'NONE',  ( -0.5609751937345790473, -0.1601694915254239793, 7.293870047334757523 ) ) ;
#15225 = EDGE_CURVE ( 'NONE', #2681, #9321, #4110, .T. ) ;
#15226 = EDGE_LOOP ( 'NONE', ( #12997, #10410, #10500, #5210 ) ) ;
#15227 = DIRECTION ( 'NONE',  ( 0.000000000000000000, 0.000000000000000000, 1.000000000000000000 ) ) ;
#15228 = CARTESIAN_POINT ( 'NONE',  ( 2.219956784870649180, -2.173136654396200740, 3.918630970161570026 ) ) ;
#15229 = CARTESIAN_POINT ( 'NONE',  ( 2.328217775191430139, -5.381991525423729605, 5.043379051721160522 ) ) ;
#15230 = CARTESIAN_POINT ( 'NONE',  ( 0.2908063684825958894, -1.055298816558370101, 7.337905485238597869 ) ) ;
#15231 = VERTEX_POINT ( 'NONE', #5499 ) ;
#15232 = CARTESIAN_POINT ( 'NONE',  ( -0.8298945877350979439, -5.211074464177370302, 2.494426474263899962 ) ) ;
#15233 = CARTESIAN_POINT ( 'NONE',  ( 1.703239418290648732, -0.5429564742160235546, 3.553755118148703929 ) ) ;
#15234 = EDGE_CURVE ( 'NONE', #8501, #12906, #4199, .T. ) ;
#15235 = CARTESIAN_POINT ( 'NONE',  ( 2.051568858000881068, -0.5196681859277345605, 3.016498023208322277 ) ) ;
#15236 = CARTESIAN_POINT ( 'NONE',  ( -1.399999999999999911, -8.000000000000000000, 6.100000000000000533 ) ) ;
#15237 = DIRECTION ( 'NONE',  ( -2.297013154396880191E-16, 1.000000000000000000, 0.000000000000000000 ) ) ;
#15238 = CARTESIAN_POINT ( 'NONE',  ( -4.898587196589392737E-17, 5.318248954186071131, 6.349999999999999645 ) ) ;
#15239 = CARTESIAN_POINT ( 'NONE',  ( 2.050994839075679366, -0.9815930753335269099, 4.608774933727144862 ) ) ;
#15240 = AXIS2_PLACEMENT_3D ( 'NONE', #11292, #16929, #11379 ) ;
#15241 = LINE ( 'NONE', #7097, #12656 ) ;
#15242 = VERTEX_POINT ( 'NONE', #9490 ) ;
#15243 = CARTESIAN_POINT ( 'NONE',  ( -1.899999999999999911, 0.5999999999999999778, 7.550000000000000711 ) ) ;
#15244 = DIRECTION ( 'NONE',  ( 0.000000000000000000, 0.000000000000000000, 1.000000000000000000 ) ) ;
#15245 = CARTESIAN_POINT ( 'NONE',  ( 2.632194480419669080, -2.289578095837640159, 5.038623552414890128 ) ) ;
#15246 = EDGE_CURVE ( 'NONE', #1331, #14447, #15149, .T. ) ;
#15247 = ORIENTED_EDGE ( 'NONE', *, *, #6540, .F. ) ;
#15248 = DIRECTION ( 'NONE',  ( 9.349246523159210481E-16, 0.000000000000000000, 1.000000000000000000 ) ) ;
#15249 = CARTESIAN_POINT ( 'NONE',  ( 1.289141334274990447, -5.417584745762705545, 6.297747079672416426 ) ) ;
#15250 = ORIENTED_EDGE ( 'NONE', *, *, #11096, .T. ) ;
#15251 = DIRECTION ( 'NONE',  ( -1.000000000000000000, 2.381191005321109844E-32, 0.000000000000000000 ) ) ;
#15252 = DIRECTION ( 'NONE',  ( 1.224646799147350002E-16, -1.000000000000000000, -6.123233995736759873E-17 ) ) ;
#15253 = CARTESIAN_POINT ( 'NONE',  ( 0.1749999999999999889, 9.099999999999999645, 0.4000000000000000222 ) ) ;
#15254 = CARTESIAN_POINT ( 'NONE',  ( 1.112838723655040107, -5.426483050847459744, 6.773667561836210105 ) ) ;
#15255 = CARTESIAN_POINT ( 'NONE',  ( 2.325590009395039903, -0.7292627805223299564, 5.061077271074021056 ) ) ;
#15256 = CARTESIAN_POINT ( 'NONE',  ( 2.105672170043351166, -3.962493976234419790, 3.084680091961101045 ) ) ;
#15257 = EDGE_CURVE ( 'NONE', #3526, #17345, #16450, .T. ) ;
#15258 = CARTESIAN_POINT ( 'NONE',  ( -1.000000000000000000, -6.000000000000000000, 3.673738709727309981 ) ) ;
#15259 = CARTESIAN_POINT ( 'NONE',  ( -0.8967027089122764361, -1.195028546288099625, 6.546842195331652903 ) ) ;
#15260 = CARTESIAN_POINT ( 'NONE',  ( -1.000000000000000000, 6.799999999999999822, 7.700000000000000178 ) ) ;
#15261 = EDGE_CURVE ( 'NONE', #7957, #16569, #15431, .T. ) ;
#15262 = LINE ( 'NONE', #8222, #4688 ) ;
#15263 = EDGE_LOOP ( 'NONE', ( #7409, #10707, #889 ) ) ;
#15264 = EDGE_CURVE ( 'NONE', #16165, #8415, #1434, .T. ) ;
#15265 = EDGE_CURVE ( 'NONE', #10426, #6674, #6806, .T. ) ;
#15266 = CARTESIAN_POINT ( 'NONE',  ( 1.685353174447271840, -5.039854330134263094, 3.014646825552728782 ) ) ;
#15267 = CARTESIAN_POINT ( 'NONE',  ( 2.560337424259670591, -0.3622881355932213721, 4.001768473655590519 ) ) ;
#15268 = ADVANCED_FACE ( 'NONE', ( #18152 ), #14017, .F. ) ;
#15269 = CARTESIAN_POINT ( 'NONE',  ( 0.3949552299394610277, -3.776187669928119828, 2.379923265530350385 ) ) ;
#15270 = CARTESIAN_POINT ( 'NONE',  ( -0.5500000000000000444, 0.5999999999999999778, 1.600000000000000089 ) ) ;
#15271 = EDGE_CURVE ( 'NONE', #4902, #6049, #10975, .T. ) ;
#15272 = CARTESIAN_POINT ( 'NONE',  ( 1.000000000000000000, -5.000000000000000000, 3.299999999999999822 ) ) ;
#15273 = CARTESIAN_POINT ( 'NONE',  ( -1.554165089654128584, -5.479872881355935199, 6.851145244874527584 ) ) ;
#15274 = EDGE_LOOP ( 'NONE', ( #8823, #11872, #16590, #7278, #5638, #3300, #6076, #17435, #6331, #3108, #9461, #40, #17536, #7230, #11487, #953, #13033, #18237 ) ) ;
#15275 = DIRECTION ( 'NONE',  ( 1.000000000000000000, 0.000000000000000000, -7.401486830834380223E-16 ) ) ;
#15276 = CARTESIAN_POINT ( 'NONE',  ( -1.978267656359408821, -5.197669491525419794, 5.974740860598791947 ) ) ;
#15277 = CARTESIAN_POINT ( 'NONE',  ( 1.899999999999999911, 11.29999999999999893, 7.649999999999999467 ) ) ;
#15278 = PLANE ( 'NONE',  #12679 ) ;
#15279 = ORIENTED_EDGE ( 'NONE', *, *, #2751, .T. ) ;
#15280 = CARTESIAN_POINT ( 'NONE',  ( 2.260890494820590124, -4.055647129387580208, 4.046455925041149371 ) ) ;
#15281 = ADVANCED_FACE ( 'NONE', ( #3924 ), #5603, .T. ) ;
#15282 = CARTESIAN_POINT ( 'NONE',  ( 0.1969988207263408952, -5.304612347394259686, 2.648915996644538584 ) ) ;
#15283 = LINE ( 'NONE', #15660, #15748 ) ;
#15284 = LINE ( 'NONE', #9624, #2579 ) ;
#15285 = CARTESIAN_POINT ( 'NONE',  ( 0.5570002967656469961, -2.891232714973159812, 6.986590552960210587 ) ) ;
#15286 = LINE ( 'NONE', #2600, #7565 ) ;
#15287 = VECTOR ( 'NONE', #16623, 1000.000000000000000 ) ;
#15288 = CARTESIAN_POINT ( 'NONE',  ( -2.049636678546640667, -3.356998480738929924, 4.582138519505405405 ) ) ;
#15289 = VECTOR ( 'NONE', #13813, 1000.000000000000000 ) ;
#15290 = ADVANCED_FACE ( 'NONE', ( #2538 ), #12629, .T. ) ;
#15291 = AXIS2_PLACEMENT_3D ( 'NONE', #883, #4755, #13282 ) ;
#15292 = CARTESIAN_POINT ( 'NONE',  ( -1.899999999999999911, -5.909399420205969064E-16, 4.000000000000000000 ) ) ;
#15293 = CARTESIAN_POINT ( 'NONE',  ( 0.4360591020457930123, -0.3088983050847460277, 2.387347919655840034 ) ) ;
#15294 = CARTESIAN_POINT ( 'NONE',  ( -1.800000000000000044, 0.5999999999999999778, 1.600000000000000089 ) ) ;
#15295 = VERTEX_POINT ( 'NONE', #18070 ) ;
#15296 = FACE_OUTER_BOUND ( 'NONE', #7834, .T. ) ;
#15297 = ORIENTED_EDGE ( 'NONE', *, *, #11207, .T. ) ;
#15298 = ORIENTED_EDGE ( 'NONE', *, *, #8512, .F. ) ;
#15299 = AXIS2_PLACEMENT_3D ( 'NONE', #15354, #16907, #2938 ) ;
#15300 = UNCERTAINTY_MEASURE_WITH_UNIT (LENGTH_MEASURE( 1.000000000000000082E-05 ), #1243, 'distance_accuracy_value', 'NONE');
#15301 = ORIENTED_EDGE ( 'NONE', *, *, #14374, .T. ) ;
#15302 = CARTESIAN_POINT ( 'NONE',  ( -0.8740908734716290596, 4.154758922476410099, 7.700000000000000178 ) ) ;
#15303 = CARTESIAN_POINT ( 'NONE',  ( -0.5137283630188880235, -5.162076271186444743, 6.687652957477222770 ) ) ;
#15304 = CARTESIAN_POINT ( 'NONE',  ( -0.9250303514741213817, -1.777235753495299608, 2.212544966868041474 ) ) ;
#15305 = TOROIDAL_SURFACE ( 'NONE', #9669, 0.2999999999999999889, 0.2500000000000000000 ) ;
#15306 = CARTESIAN_POINT ( 'NONE',  ( -1.289999999999999813, 4.099999999999998757, 1.106527474781921491E-15 ) ) ;
#15307 = CIRCLE ( 'NONE', #11445, 0.04999999999999969746 ) ;
#15308 = LINE ( 'NONE', #5577, #13223 ) ;
#15309 = CARTESIAN_POINT ( 'NONE',  ( -1.850000000000000089, 11.25000000000000000, 8.300000000000000711 ) ) ;
#15310 = LINE ( 'NONE', #11222, #10013 ) ;
#15311 = VECTOR ( 'NONE', #17281, 1000.000000000000000 ) ;
#15312 = DIRECTION ( 'NONE',  ( 0.000000000000000000, 1.000000000000000000, 2.775557561562890365E-16 ) ) ;
#15313 = CARTESIAN_POINT ( 'NONE',  ( 1.000000000000000000, -5.500000000000000000, 6.100000000000000533 ) ) ;
#15314 = CARTESIAN_POINT ( 'NONE',  ( 2.226511124464869873, -1.074746228486680000, 5.462491901673799610 ) ) ;
#15315 =( GEOMETRIC_REPRESENTATION_CONTEXT ( 3 ) GLOBAL_UNCERTAINTY_ASSIGNED_CONTEXT ( ( #1038 ) ) GLOBAL_UNIT_ASSIGNED_CONTEXT ( ( #15942, #16028, #4446 ) ) REPRESENTATION_CONTEXT ( 'NONE', 'WORKASPACE' ) );
#15316 = CARTESIAN_POINT ( 'NONE',  ( -2.020286629067959971, -0.1913135593220339215, 6.420841923842841581 ) ) ;
#15317 = EDGE_CURVE ( 'NONE', #7434, #9192, #5416, .T. ) ;
#15318 = CARTESIAN_POINT ( 'NONE',  ( -1.399999999999999911, -5.500000000000000000, 5.100000000000000533 ) ) ;
#15319 = VERTEX_POINT ( 'NONE', #8467 ) ;
#15320 = AXIS2_PLACEMENT_3D ( 'NONE', #343, #7382, #15892 ) ;
#15321 = CARTESIAN_POINT ( 'NONE',  ( -1.873832970144350130, -0.2625000000000002331, 2.826167029855650270 ) ) ;
#15322 = VECTOR ( 'NONE', #17169, 1000.000000000000000 ) ;
#15323 = LINE ( 'NONE', #16692, #2444 ) ;
#15324 = VERTEX_POINT ( 'NONE', #4011 ) ;
#15325 = CARTESIAN_POINT ( 'NONE',  ( -0.3042893218813459977, 3.050000000000000266, 2.170710678118660031 ) ) ;
#15326 = CARTESIAN_POINT ( 'NONE',  ( -0.6096110657044611081, -1.800524041783590157, 2.426869991387521353 ) ) ;
#15327 = SHAPE_REPRESENTATION_RELATIONSHIP ( 'NONE' , 'NONE' ,  #8322, #4434 ) ;
#15328 = CARTESIAN_POINT ( 'NONE',  ( -0.2189795514005259958, -5.595550847457629651, 2.356806637999020015 ) ) ;
#15329 = VECTOR ( 'NONE', #6083, 1000.000000000000000 ) ;
#15330 = VECTOR ( 'NONE', #1435, 1000.000000000000000 ) ;
#15331 = ORIENTED_EDGE ( 'NONE', *, *, #16845, .T. ) ;
#15332 = CARTESIAN_POINT ( 'NONE',  ( 2.145694642186089851, -1.098034516774969882, 5.666819626392539888 ) ) ;
#15333 = CARTESIAN_POINT ( 'NONE',  ( -1.480680413335760059, -4.385524041783589233, 6.529298007719829933 ) ) ;
#15334 = ORIENTED_EDGE ( 'NONE', *, *, #1042, .F. ) ;
#15335 = AXIS2_PLACEMENT_3D ( 'NONE', #2835, #4126, #1264 ) ;
#15336 = LINE ( 'NONE', #17885, #1679 ) ;
#15337 = DIRECTION ( 'NONE',  ( -0.000000000000000000, 1.000000000000000000, 0.000000000000000000 ) ) ;
#15338 = DIRECTION ( 'NONE',  ( -8.163404592832159998E-18, -1.000000000000000000, 0.000000000000000000 ) ) ;
#15339 = CARTESIAN_POINT ( 'NONE',  ( 1.292934267244360447, -1.214475958216409746, 6.294748514096617065 ) ) ;
#15340 = LINE ( 'NONE', #2647, #12939 ) ;
#15341 = EDGE_LOOP ( 'NONE', ( #14065, #3752, #2278, #99 ) ) ;
#15342 = DIRECTION ( 'NONE',  ( -1.000000000000000000, 7.401486830834380223E-16, 0.000000000000000000 ) ) ;
#15343 = DIRECTION ( 'NONE',  ( 0.000000000000000000, 6.123233995736769734E-17, -1.000000000000000000 ) ) ;
#15344 = AXIS2_PLACEMENT_3D ( 'NONE', #2119, #6364, #636 ) ;
#15345 = CARTESIAN_POINT ( 'NONE',  ( -1.679950111053631900, -0.1957627118644069686, 5.880020650119711867 ) ) ;
#15346 = VECTOR ( 'NONE', #16489, 1000.000000000000000 ) ;
#15347 = CARTESIAN_POINT ( 'NONE',  ( 0.2266049403549809660, -3.453992510252061887, 2.055805624767989226 ) ) ;
#15348 = CARTESIAN_POINT ( 'NONE',  ( -0.1686436619862690112, -4.981295943764799894, 2.349239845786320391 ) ) ;
#15349 = CARTESIAN_POINT ( 'NONE',  ( 0.2453710345350221533, -5.144279661016955885, 6.738252723719333481 ) ) ;
#15350 = ORIENTED_EDGE ( 'NONE', *, *, #2059, .F. ) ;
#15351 = AXIS2_PLACEMENT_3D ( 'NONE', #2145, #13439, #10294 ) ;
#15352 = PLANE ( 'NONE',  #2079 ) ;
#15353 = CARTESIAN_POINT ( 'NONE',  ( 1.713314936023349944, -5.338983050847460277, 3.089913064446569546 ) ) ;
#15354 = CARTESIAN_POINT ( 'NONE',  ( -1.875000000000000000, 12.00000000000000000, 7.700000000000000178 ) ) ;
#15355 = VERTEX_POINT ( 'NONE', #2643 ) ;
#15356 = CARTESIAN_POINT ( 'NONE',  ( -1.428515267734880023, -5.568855932203390147, 2.829745655876930055 ) ) ;
#15357 = AXIS2_PLACEMENT_3D ( 'NONE', #3109, #6067, #4678 ) ;
#15358 = VECTOR ( 'NONE', #10182, 1000.000000000000000 ) ;
#15359 = CARTESIAN_POINT ( 'NONE',  ( 2.334748642087659753, -0.6593979156574649725, 4.403867486184820379 ) ) ;
#15360 = CARTESIAN_POINT ( 'NONE',  ( 0.2010642693393740188, -3.752899381639833720, 2.053740970237999619 ) ) ;
#15361 = DIRECTION ( 'NONE',  ( 4.037174635000570090E-16, -1.000000000000000000, 4.482164234210289821E-32 ) ) ;
#15362 = CARTESIAN_POINT ( 'NONE',  ( 2.036910256464071090, -0.6593979156574641953, 4.443293066459086837 ) ) ;
#15363 = DIRECTION ( 'NONE',  ( 1.000000000000000000, 0.000000000000000000, 0.000000000000000000 ) ) ;
#15364 = AXIS2_PLACEMENT_3D ( 'NONE', #12531, #9657, #18144 ) ;
#15365 = ORIENTED_EDGE ( 'NONE', *, *, #5359, .F. ) ;
#15366 = DIRECTION ( 'NONE',  ( 1.000000000000000000, 0.000000000000000000, 0.000000000000000000 ) ) ;
#15367 = CARTESIAN_POINT ( 'NONE',  ( 0.7322514394120266390, -0.3133474576271193524, 2.149183891723918993 ) ) ;
#15368 = CARTESIAN_POINT ( 'NONE',  ( 1.526791597786429922, -2.774791273531720392, 6.490992212270249695 ) ) ;
#15369 = DIRECTION ( 'NONE',  ( 0.000000000000000000, -2.220446049250309876E-16, 1.000000000000000000 ) ) ;
#15370 = CARTESIAN_POINT ( 'NONE',  ( -7.347880794884118997E-17, 0.5999999999999999778, 3.673940397442059498E-17 ) ) ;
#15371 = CARTESIAN_POINT ( 'NONE',  ( -1.925836318347889931, -5.488771186440680516, 6.525927015348141680 ) ) ;
#15372 = ORIENTED_EDGE ( 'NONE', *, *, #13322, .F. ) ;
#15373 = ORIENTED_EDGE ( 'NONE', *, *, #556, .F. ) ;
#15374 = LINE ( 'NONE', #1564, #13641 ) ;
#15375 = DIRECTION ( 'NONE',  ( 1.000000000000000000, 0.000000000000000000, 0.000000000000000000 ) ) ;
#15376 = CARTESIAN_POINT ( 'NONE',  ( -1.889999999999999902, 7.900000000000000355, 0.5999999999999999778 ) ) ;
#15377 = PRODUCT_DEFINITION_FORMATION_WITH_SPECIFIED_SOURCE ( 'ANY', '', #1066, .NOT_KNOWN. ) ;
#15378 = EDGE_CURVE ( 'NONE', #16660, #2515, #8293, .T. ) ;
#15379 = VERTEX_POINT ( 'NONE', #12541 ) ;
#15380 = CARTESIAN_POINT ( 'NONE',  ( -2.349464193210359930, -3.356998480738930368, 4.563019372514619754 ) ) ;
#15381 = EDGE_CURVE ( 'NONE', #2742, #9183, #15699, .T. ) ;
#15382 = PRESENTATION_STYLE_ASSIGNMENT (( #1481 ) ) ;
#15383 = CARTESIAN_POINT ( 'NONE',  ( 1.449568901432419343, -5.337500000000000355, 3.250431098567584165 ) ) ;
#15384 = ADVANCED_FACE ( 'NONE', ( #10127 ), #14297, .T. ) ;
#15385 = AXIS2_PLACEMENT_3D ( 'NONE', #9666, #8384, #9948 ) ;
#15386 = FACE_OUTER_BOUND ( 'NONE', #12028, .T. ) ;
#15387 = ADVANCED_FACE ( 'NONE', ( #405 ), #4469, .F. ) ;
#15388 = DIRECTION ( 'NONE',  ( 0.000000000000000000, 1.000000000000000000, 0.000000000000000000 ) ) ;
#15389 = CARTESIAN_POINT ( 'NONE',  ( 1.728413393879709936, -4.311818300558750039, 6.297289212178290185 ) ) ;
#15390 = CARTESIAN_POINT ( 'NONE',  ( -1.899999999999999911, -2.607830583485250056E-17, -4.440892098500630106E-16 ) ) ;
#15391 = CARTESIAN_POINT ( 'NONE',  ( -0.9976707306414490661, -3.077539021279473097, 6.494311833503151554 ) ) ;
#15392 = DIRECTION ( 'NONE',  ( -6.123233995736774664E-17, 0.000000000000000000, -1.000000000000000000 ) ) ;
#15393 = ORIENTED_EDGE ( 'NONE', *, *, #15794, .T. ) ;
#15394 = DIRECTION ( 'NONE',  ( 0.000000000000000000, 0.000000000000000000, 1.000000000000000000 ) ) ;
#15395 = ORIENTED_EDGE ( 'NONE', *, *, #11175, .T. ) ;
#15396 = CARTESIAN_POINT ( 'NONE',  ( -1.626408692231610109, -4.707719201459649838, 6.401040991074980369 ) ) ;
#15397 = VERTEX_POINT ( 'NONE', #6044 ) ;
#15398 = CIRCLE ( 'NONE', #15972, 0.4166666666666669072 ) ;
#15399 = ORIENTED_EDGE ( 'NONE', *, *, #8370, .F. ) ;
#15400 = CARTESIAN_POINT ( 'NONE',  ( -1.875000000000000000, 0.7500000000000000000, 7.700000000000000178 ) ) ;
#15401 = ORIENTED_EDGE ( 'NONE', *, *, #4824, .F. ) ;
#15402 = LINE ( 'NONE', #3986, #11491 ) ;
#15403 = CARTESIAN_POINT ( 'NONE',  ( -0.8731223871104993872, -5.170974576271189171, 6.558046933601121786 ) ) ;
#15404 = CARTESIAN_POINT ( 'NONE',  ( 2.008025181017630167, -2.079983501243050981, 2.964791492240490101 ) ) ;
#15405 = ADVANCED_FACE ( 'NONE', ( #321 ), #11425, .T. ) ;
#15406 = DIRECTION ( 'NONE',  ( -1.000000000000000000, 0.000000000000000000, 0.000000000000000000 ) ) ;
#15407 = CARTESIAN_POINT ( 'NONE',  ( -0.1749999999999999889, 9.500000000000000000, 3.100000000000000089 ) ) ;
#15408 = DIRECTION ( 'NONE',  ( 1.000000000000000000, 9.697257589008697037E-16, 0.000000000000000000 ) ) ;
#15409 = CARTESIAN_POINT ( 'NONE',  ( -2.500000000000000000, 7.299999999999999822, 0.6099999999999999867 ) ) ;
#15410 = FACE_OUTER_BOUND ( 'NONE', #9527, .T. ) ;
#15411 = VECTOR ( 'NONE', #11609, 1000.000000000000000 ) ;
#15412 = CARTESIAN_POINT ( 'NONE',  ( 1.704669856830330010, -0.8030495317899829510, 3.080704711052640210 ) ) ;
#15413 = CARTESIAN_POINT ( 'NONE',  ( 0.8259795455966094657, -2.545749267008810435, 6.579537079411867495 ) ) ;
#15414 = CARTESIAN_POINT ( 'NONE',  ( 1.647941990407678636, -0.04449152542372906277, 3.475676388127089123 ) ) ;
#15415 = ORIENTED_EDGE ( 'NONE', *, *, #5419, .F. ) ;
#15416 = CARTESIAN_POINT ( 'NONE',  ( -2.224278379903029901, -0.5091101694915259879, 5.468825643806110470 ) ) ;
#15417 = ORIENTED_EDGE ( 'NONE', *, *, #9140, .T. ) ;
#15418 = CARTESIAN_POINT ( 'NONE',  ( 0.3743405594629510280, -0.1423728813559329842, 7.023440622744399953 ) ) ;
#15419 = CARTESIAN_POINT ( 'NONE',  ( 1.115198193348289957, -1.261052534792989954, 6.772457159276550342 ) ) ;
#15420 = ORIENTED_EDGE ( 'NONE', *, *, #17393, .T. ) ;
#15421 = CARTESIAN_POINT ( 'NONE',  ( 1.899999999999999911, 7.299999999999999822, 1.600000000000000089 ) ) ;
#15422 = ORIENTED_EDGE ( 'NONE', *, *, #14042, .T. ) ;
#15423 = CARTESIAN_POINT ( 'NONE',  ( 2.237394498046679558, -2.336154672414219924, 5.429939413646329704 ) ) ;
#15424 = VECTOR ( 'NONE', #10423, 1000.000000000000114 ) ;
#15425 = CARTESIAN_POINT ( 'NONE',  ( 2.020286629067969297, -5.408686440677975327, 6.420841923842827370 ) ) ;
#15426 = EDGE_CURVE ( 'NONE', #6584, #17750, #1952, .T. ) ;
#15427 = ORIENTED_EDGE ( 'NONE', *, *, #8297, .T. ) ;
#15428 = CARTESIAN_POINT ( 'NONE',  ( -2.255259958075430227, -1.703530012270459970, 5.372717034856060003 ) ) ;
#15429 = CARTESIAN_POINT ( 'NONE',  ( -1.949083719010310078, -0.5402542372881364852, 4.055210292801460170 ) ) ;
#15430 = VERTEX_POINT ( 'NONE', #8565 ) ;
#15431 = LINE ( 'NONE', #2737, #16752 ) ;
#15432 = CARTESIAN_POINT ( 'NONE',  ( 1.192893218813449785, -10.00000000000000000, 3.507106781186551725 ) ) ;
#15433 = PLANE ( 'NONE',  #15385 ) ;
#15434 = CARTESIAN_POINT ( 'NONE',  ( -2.021195349941399044, -1.819971453711898945, 4.339901124684693912 ) ) ;
#15435 = LINE ( 'NONE', #8386, #8212 ) ;
#15436 = ORIENTED_EDGE ( 'NONE', *, *, #16825, .F. ) ;
#15437 = CARTESIAN_POINT ( 'NONE',  ( -1.289999999999999813, 4.099999999999998757, 0.6000000000000017542 ) ) ;
#15438 = CARTESIAN_POINT ( 'NONE',  ( -1.899999999999999911, 2.799999999999999822, 1.600000000000000089 ) ) ;
#15439 = CARTESIAN_POINT ( 'NONE',  ( 2.644456467089558949, -3.803316834576382366, 4.476474416072626639 ) ) ;
#15440 = CARTESIAN_POINT ( 'NONE',  ( -0.1749999999999999889, 7.700000000000000178, 1.600000000000000089 ) ) ;
#15441 = CARTESIAN_POINT ( 'NONE',  ( -0.1881942810071039751, -5.280843314568230085, 2.350674491507239949 ) ) ;
#15442 = CARTESIAN_POINT ( 'NONE',  ( 1.880631435828169939, -5.355296610169490101, 3.876649216148224220 ) ) ;
#15443 = ORIENTED_EDGE ( 'NONE', *, *, #3722, .T. ) ;
#15444 = CARTESIAN_POINT ( 'NONE',  ( 2.306642602145299925, -0.08453389830508534208, 5.166805192608479480 ) ) ;
#15445 = DIRECTION ( 'NONE',  ( -3.700743415417190112E-16, -1.000000000000000000, -9.251858538542959255E-17 ) ) ;
#15446 = CARTESIAN_POINT ( 'NONE',  ( 3.591599821218572011E-17, 3.615866958331936942, 7.736552763412142042 ) ) ;
#15447 = ADVANCED_FACE ( 'NONE', ( #14212 ), #15609, .T. ) ;
#15448 = EDGE_LOOP ( 'NONE', ( #3295, #1131, #6305, #10403 ) ) ;
#15449 = LINE ( 'NONE', #11359, #18215 ) ;
#15450 = CARTESIAN_POINT ( 'NONE',  ( -1.724579595320040015, -1.660794312053859967, 3.098572228637930248 ) ) ;
#15451 = DIRECTION ( 'NONE',  ( 1.306144734853129823E-16, -1.000000000000000000, 0.000000000000000000 ) ) ;
#15452 = CARTESIAN_POINT ( 'NONE',  ( -2.329383452786330189, -4.571830348089889640, 5.035735636132879556 ) ) ;
#15453 = FACE_OUTER_BOUND ( 'NONE', #1099, .T. ) ;
#15454 = ORIENTED_EDGE ( 'NONE', *, *, #11572, .T. ) ;
#15455 = LINE ( 'NONE', #2763, #14438 ) ;
#15456 = CARTESIAN_POINT ( 'NONE',  ( 2.268288188848061715, -0.3489406779661023417, 3.322421079292310786 ) ) ;
#15457 = CARTESIAN_POINT ( 'NONE',  ( -1.097561405233230092, -3.613169651910099756, 2.618148744692269769 ) ) ;
#15458 = DIRECTION ( 'NONE',  ( 1.224646799147350002E-16, -1.000000000000000000, -6.123233995736769734E-17 ) ) ;
#15459 = PLANE ( 'NONE',  #6502 ) ;
#15460 = CARTESIAN_POINT ( 'NONE',  ( 2.191755591049679541, -5.046398305084744962, 3.203650300307709475 ) ) ;
#15461 = ORIENTED_EDGE ( 'NONE', *, *, #11762, .F. ) ;
#15462 = ADVANCED_FACE ( 'NONE', ( #10044 ), #1706, .T. ) ;
#15463 = CARTESIAN_POINT ( 'NONE',  ( -0.2189795514005259958, -5.295550847457628940, 2.356806637999020015 ) ) ;
#15464 = DIRECTION ( 'NONE',  ( 1.110223024625159992E-16, 0.000000000000000000, -1.000000000000000000 ) ) ;
#15465 = EDGE_LOOP ( 'NONE', ( #17902, #3655, #7475, #18084 ) ) ;
#15466 = CARTESIAN_POINT ( 'NONE',  ( -2.239137794397029868, -4.987178660919110662, 3.975425900939220103 ) ) ;
#15467 = CARTESIAN_POINT ( 'NONE',  ( 1.526064881623949931, -0.7763906680874419486, 2.903976516638540062 ) ) ;
#15468 = VECTOR ( 'NONE', #5963, 1000.000000000000000 ) ;
#15469 = CARTESIAN_POINT ( 'NONE',  ( 0.2134934900267039248, -5.004947479095229745, 2.650814970067049803 ) ) ;
#15470 = LINE ( 'NONE', #3972, #11556 ) ;
#15471 = DIRECTION ( 'NONE',  ( 0.000000000000000000, 0.000000000000000000, -1.000000000000000000 ) ) ;
#15472 = CARTESIAN_POINT ( 'NONE',  ( -1.917298190932639868, -3.496728210468659892, 3.335187436117939885 ) ) ;
#15473 = CARTESIAN_POINT ( 'NONE',  ( -1.875000000000000000, 0.7500000000000000000, 7.700000000000000178 ) ) ;
#15474 = CARTESIAN_POINT ( 'NONE',  ( 1.366362128262241571, -3.915917399657852904, 3.167695729602394206 ) ) ;
#15475 = ORIENTED_EDGE ( 'NONE', *, *, #9718, .F. ) ;
#15476 = DIRECTION ( 'NONE',  ( 1.000000000000000000, 0.000000000000000000, 1.850371707708589879E-16 ) ) ;
#15477 = VERTEX_POINT ( 'NONE', #14562 ) ;
#15478 = EDGE_CURVE ( 'NONE', #5150, #6911, #11340, .T. ) ;
#15479 = CARTESIAN_POINT ( 'NONE',  ( -1.899999999999999911, 0.5999999999999999778, 1.600000000000000089 ) ) ;
#15480 = ORIENTED_EDGE ( 'NONE', *, *, #6879, .F. ) ;
#15481 = ADVANCED_FACE ( 'NONE', ( #13088 ), #51, .F. ) ;
#15482 = EDGE_LOOP ( 'NONE', ( #8970, #11531, #14152, #18249 ) ) ;
#15483 = CARTESIAN_POINT ( 'NONE',  ( 2.500000000000000000, 2.000000000000000000, 1.600000000000000089 ) ) ;
#15484 = UNCERTAINTY_MEASURE_WITH_UNIT (LENGTH_MEASURE( 1.000000000000000082E-05 ), #10944, 'distance_accuracy_value', 'NONE');
#15485 = ORIENTED_EDGE ( 'NONE', *, *, #16197, .F. ) ;
#15486 = DIRECTION ( 'NONE',  ( -1.000000000000000000, 0.000000000000000000, 4.440892098500620245E-16 ) ) ;
#15487 = CARTESIAN_POINT ( 'NONE',  ( -1.725722849164588624, -5.197669491525426011, 5.812007984777676661 ) ) ;
#15488 = DIRECTION ( 'NONE',  ( 4.440892098500620245E-16, -1.000000000000000000, 0.000000000000000000 ) ) ;
#15489 = CARTESIAN_POINT ( 'NONE',  ( 1.681140935901590083, -0.7917284067793100011, 3.001197262379470043 ) ) ;
#15490 = DIRECTION ( 'NONE',  ( -1.531342102931250010E-16, 1.000000000000000000, 0.000000000000000000 ) ) ;
#15491 = FACE_OUTER_BOUND ( 'NONE', #1789, .T. ) ;
#15492 = CARTESIAN_POINT ( 'NONE',  ( 1.444955263746720009, -2.332313796054249710, 2.842353646881480511 ) ) ;
#15493 = CARTESIAN_POINT ( 'NONE',  ( -1.854389246811851022, -3.151244762504313179, 3.819010576716904026 ) ) ;
#15494 = CARTESIAN_POINT ( 'NONE',  ( 2.046424002475610404, -0.07118644067796651986, 4.536201610417760044 ) ) ;
#15495 = EDGE_CURVE ( 'NONE', #9165, #7939, #17147, .T. ) ;
#15496 = ORIENTED_EDGE ( 'NONE', *, *, #14723, .F. ) ;
#15497 = CARTESIAN_POINT ( 'NONE',  ( 1.851073041990159984, -0.4067796610169499560, 6.153284478378259870 ) ) ;
#15498 = EDGE_CURVE ( 'NONE', #11926, #13468, #2562, .T. ) ;
#15499 = FACE_OUTER_BOUND ( 'NONE', #9821, .T. ) ;
#15500 = VERTEX_POINT ( 'NONE', #1803 ) ;
#15501 = EDGE_CURVE ( 'NONE', #5857, #15295, #8734, .T. ) ;
#15502 = CARTESIAN_POINT ( 'NONE',  ( 1.194742379459969861, -0.1245762711864410038, 6.727584234649759409 ) ) ;
#15503 = CARTESIAN_POINT ( 'NONE',  ( 1.794646911016580137, -1.167899381639829981, 6.222494056560660347 ) ) ;
#15504 = VECTOR ( 'NONE', #18121, 999.9999999999998863 ) ;
#15505 = ORIENTED_EDGE ( 'NONE', *, *, #17143, .F. ) ;
#15506 = EDGE_CURVE ( 'NONE', #2878, #2905, #7181, .T. ) ;
#15507 = ADVANCED_BREP_SHAPE_REPRESENTATION ( '', ( #14083, #17681 ), #3818 ) ;
#15508 = EDGE_CURVE ( 'NONE', #10505, #8570, #12821, .T. ) ;
#15509 = ORIENTED_EDGE ( 'NONE', *, *, #17305, .F. ) ;
#15510 = CARTESIAN_POINT ( 'NONE',  ( 0.4790341583531377845, -1.916965483225030020, 2.395814251711721354 ) ) ;
#15511 =( NAMED_UNIT ( * ) PLANE_ANGLE_UNIT ( ) SI_UNIT ( $, .RADIAN. ) );
#15512 = CARTESIAN_POINT ( 'NONE',  ( -1.554165089654128584, -5.479872881355935199, 6.851145244874527584 ) ) ;
#15513 = ORIENTED_EDGE ( 'NONE', *, *, #10583, .F. ) ;
#15514 = CARTESIAN_POINT ( 'NONE',  ( 2.291237445532070094, -0.9350164987569499209, 4.162434510291790346 ) ) ;
#15515 = CARTESIAN_POINT ( 'NONE',  ( 2.046424002475610404, -0.3711864406779670222, 4.536201610417760044 ) ) ;
#15516 = ORIENTED_EDGE ( 'NONE', *, *, #16592, .T. ) ;
#15517 = DIRECTION ( 'NONE',  ( 1.734723475976809806E-16, -1.000000000000000000, -1.387778780781449866E-16 ) ) ;
#15518 = LINE ( 'NONE', #12822, #15330 ) ;
#15519 = CARTESIAN_POINT ( 'NONE',  ( 0.5500000000000000444, 7.799999999999999822, 3.600000000000000089 ) ) ;
#15520 = MECHANICAL_DESIGN_GEOMETRIC_PRESENTATION_REPRESENTATION (  '', ( #8692 ), #3362 ) ;
#15521 = CARTESIAN_POINT ( 'NONE',  ( -0.3681613504765444134, -2.122719201459649874, 2.680257674196191431 ) ) ;
#15522 = CARTESIAN_POINT ( 'NONE',  ( 1.800000000000000044, 11.40000000000000036, 7.550000000000000711 ) ) ;
#15523 = CARTESIAN_POINT ( 'NONE',  ( 2.087380238839969593, -0.4067796610169500116, 6.338810156469096846 ) ) ;
#15524 = ORIENTED_EDGE ( 'NONE', *, *, #741, .T. ) ;
#15525 = LINE ( 'NONE', #8388, #9549 ) ;
#15526 = CARTESIAN_POINT ( 'NONE',  ( 1.836970198721030057E-17, 2.299999999999999822, 7.700000000000000178 ) ) ;
#15527 = CARTESIAN_POINT ( 'NONE',  ( 1.042222075699120287, -0.4245762711864407013, 6.468743694056166227 ) ) ;
#15528 = ADVANCED_FACE ( 'NONE', ( #3274 ), #133, .T. ) ;
#15529 = DIRECTION ( 'NONE',  ( 0.000000000000000000, 0.000000000000000000, 1.000000000000000000 ) ) ;
#15530 = CARTESIAN_POINT ( 'NONE',  ( -1.889999999999999902, 4.100000000000000533, 3.000000000000000000 ) ) ;
#15531 = CARTESIAN_POINT ( 'NONE',  ( 0.6187874668174475623, -5.135381355932194580, 6.657494107589526422 ) ) ;
#15532 = ORIENTED_EDGE ( 'NONE', *, *, #3937, .F. ) ;
#15533 = PLANE ( 'NONE',  #8317 ) ;
#15534 = CARTESIAN_POINT ( 'NONE',  ( 2.350067830300900162, -5.377542372881360500, 4.825253242917690422 ) ) ;
#15535 = FACE_OUTER_BOUND ( 'NONE', #3020, .T. ) ;
#15536 = ORIENTED_EDGE ( 'NONE', *, *, #11591, .T. ) ;
#15537 = DIRECTION ( 'NONE',  ( 1.387778780781449866E-16, 0.000000000000000000, 1.000000000000000000 ) ) ;
#15538 = CARTESIAN_POINT ( 'NONE',  ( 0.8986180677147459495, -1.963542059801610229, 2.524860635301609868 ) ) ;
#15539 = ADVANCED_FACE ( 'NONE', ( #13170 ), #17845, .T. ) ;
#15540 = CARTESIAN_POINT ( 'NONE',  ( 0.5500000000000000444, -2.399999999999999911, 3.600000000000000089 ) ) ;
#15541 = CARTESIAN_POINT ( 'NONE',  ( 0.5972539422562040956, -1.008722239981790558, 6.664227474374466276 ) ) ;
#15542 = CARTESIAN_POINT ( 'NONE',  ( 1.250000000000000000, 0.5999999999999999778, 6.100000000000000533 ) ) ;
#15543 = ORIENTED_EDGE ( 'NONE', *, *, #16987, .F. ) ;
#15544 = EDGE_CURVE ( 'NONE', #2437, #13650, #17502, .T. ) ;
#15545 = DIRECTION ( 'NONE',  ( 0.000000000000000000, 0.000000000000000000, 1.000000000000000000 ) ) ;
#15546 = CARTESIAN_POINT ( 'NONE',  ( -2.328217775191430139, -0.5180084745762719711, 5.043379051721170292 ) ) ;
#15547 = DIRECTION ( 'NONE',  ( -2.220446049250309876E-16, -1.000000000000000000, -1.479114197289400113E-30 ) ) ;
#15548 = FACE_OUTER_BOUND ( 'NONE', #13982, .T. ) ;
#15549 = CARTESIAN_POINT ( 'NONE',  ( -1.747582379783008788, -5.484322033898315851, 6.697200745122486865 ) ) ;
#15550 = ORIENTED_EDGE ( 'NONE', *, *, #881, .T. ) ;
#15551 = VERTEX_POINT ( 'NONE', #1115 ) ;
#15552 = CARTESIAN_POINT ( 'NONE',  ( -1.750316316486840051, -5.259957627118649448, 3.126818518378589928 ) ) ;
#15553 = LINE ( 'NONE', #4234, #18286 ) ;
#15554 = FACE_OUTER_BOUND ( 'NONE', #1881, .T. ) ;
#15555 = ORIENTED_EDGE ( 'NONE', *, *, #7807, .F. ) ;
#15556 = CARTESIAN_POINT ( 'NONE',  ( -1.132648842710420656, -1.493935417675870791, 7.100045893750492887 ) ) ;
#15557 = DIRECTION ( 'NONE',  ( 1.000000000000000000, 1.776356839400250070E-15, 0.000000000000000000 ) ) ;
#15558 = DIRECTION ( 'NONE',  ( -1.708035422500239940E-16, 1.000000000000000000, 8.540177112501209562E-17 ) ) ;
#15559 = CARTESIAN_POINT ( 'NONE',  ( -2.626509418457480649, -4.571830348089889640, 5.080213055741825023 ) ) ;
#15560 = LINE ( 'NONE', #537, #4917 ) ;
#15561 = CARTESIAN_POINT ( 'NONE',  ( 0.8242394280877100021, -4.428259742000189902, 6.904399023015010073 ) ) ;
#15562 = DIRECTION ( 'NONE',  ( 0.000000000000000000, 0.000000000000000000, 1.000000000000000000 ) ) ;
#15563 = CARTESIAN_POINT ( 'NONE',  ( 0.1086361371091010830, -2.937809291549738688, 6.750146344128172160 ) ) ;
#15564 = DIRECTION ( 'NONE',  ( 0.000000000000000000, -1.000000000000000000, -6.167905692361979821E-17 ) ) ;
#15565 = ORIENTED_EDGE ( 'NONE', *, *, #1894, .T. ) ;
#15566 = CARTESIAN_POINT ( 'NONE',  ( -0.4037348727536037574, -0.5906145504024216120, 2.679104755345550704 ) ) ;
#15567 = VERTEX_POINT ( 'NONE', #4821 ) ;
#15568 = AXIS2_PLACEMENT_3D ( 'NONE', #14170, #5559, #7145 ) ;
#15569 =( NAMED_UNIT ( * ) SI_UNIT ( $, .STERADIAN. ) SOLID_ANGLE_UNIT ( ) );
#15570 = ORIENTED_EDGE ( 'NONE', *, *, #1236, .F. ) ;
#15571 = LINE ( 'NONE', #7318, #4921 ) ;
#15572 = CARTESIAN_POINT ( 'NONE',  ( -0.1749999999999999889, 8.200000000000001066, -3.200000000000000178 ) ) ;
#15573 = ORIENTED_EDGE ( 'NONE', *, *, #15735, .T. ) ;
#15574 = CARTESIAN_POINT ( 'NONE',  ( -1.614765845140348821, -5.193220338983044471, 5.967758800287426446 ) ) ;
#15575 = CARTESIAN_POINT ( 'NONE',  ( -1.769056124370508964, -1.684082600342149627, 2.721729512470790979 ) ) ;
#15576 = DIRECTION ( 'NONE',  ( -0.2800000000000001377, 0.9599999999999999645, 0.000000000000000000 ) ) ;
#15577 = FACE_OUTER_BOUND ( 'NONE', #3462, .T. ) ;
#15578 = DIRECTION ( 'NONE',  ( 2.220446049250309876E-16, 1.000000000000000000, -5.551115123125800057E-15 ) ) ;
#15579 = CARTESIAN_POINT ( 'NONE',  ( -5.204748896376249466E-17, 6.750000000000000000, 6.299999999999999822 ) ) ;
#15580 = CLOSED_SHELL ( 'NONE', ( #1312, #10491, #13595, #439, #239, #14220, #7090, #6511, #12546, #17713, #15936, #11638, #3348, #8036, #7061, #2667 ) ) ;
#15581 = VECTOR ( 'NONE', #4648, 1000.000000000000000 ) ;
#15582 = CARTESIAN_POINT ( 'NONE',  ( -1.899999999999999911, 0.5999999999999999778, 7.700000000000000178 ) ) ;
#15583 = CARTESIAN_POINT ( 'NONE',  ( 1.399999999999999911, -8.000000000000000000, 3.299999999999999822 ) ) ;
#15584 = EDGE_CURVE ( 'NONE', #1696, #9534, #10388, .T. ) ;
#15585 = CARTESIAN_POINT ( 'NONE',  ( -2.349464193210359930, -3.356998480738930368, 4.563019372514619754 ) ) ;
#15586 = CARTESIAN_POINT ( 'NONE',  ( 0.1781895581254300809, -3.453992510252061887, 2.654724878163539969 ) ) ;
#15587 = CARTESIAN_POINT ( 'NONE',  ( 1.980638384804650931, -0.06228813559322075172, 4.159858630563753934 ) ) ;
#15588 = CARTESIAN_POINT ( 'NONE',  ( -0.0009602353114128930152, -5.165218916585829767, 2.501032900279580140 ) ) ;
#15589 = DIRECTION ( 'NONE',  ( 6.123233995736769734E-17, -1.368455531567203867E-48, 1.000000000000000000 ) ) ;
#15590 = ORIENTED_EDGE ( 'NONE', *, *, #8897, .F. ) ;
#15591 = CARTESIAN_POINT ( 'NONE',  ( -0.6343239990445920240, -2.099430913171359769, 2.433641963034089972 ) ) ;
#15592 = ORIENTED_EDGE ( 'NONE', *, *, #7921, .F. ) ;
#15593 = CIRCLE ( 'NONE', #5792, 0.2000000000000000111 ) ;
#15594 = CIRCLE ( 'NONE', #16467, 0.6099999999999999867 ) ;
#15595 = EDGE_LOOP ( 'NONE', ( #2190, #7651, #8352, #10175 ) ) ;
#15596 = VECTOR ( 'NONE', #10430, 1000.000000000000000 ) ;
#15597 = CARTESIAN_POINT ( 'NONE',  ( -0.1768565782246519502, -1.847100618360170365, 2.353200596935780098 ) ) ;
#15598 =( NAMED_UNIT ( * ) PLANE_ANGLE_UNIT ( ) SI_UNIT ( $, .RADIAN. ) );
#15599 = CARTESIAN_POINT ( 'NONE',  ( -2.087380238839969593, -5.493220338983046069, 6.338810156469112833 ) ) ;
#15600 = TOROIDAL_SURFACE ( 'NONE', #15878, 0.2999999999999999889, 0.2500000000000000000 ) ;
#15601 = ORIENTED_EDGE ( 'NONE', *, *, #8733, .T. ) ;
#15602 = EDGE_CURVE ( 'NONE', #12793, #8985, #9957, .T. ) ;
#15603 = CARTESIAN_POINT ( 'NONE',  ( 2.046174187462399985, -1.121322805063259986, 5.862719605943959245 ) ) ;
#15604 = VECTOR ( 'NONE', #1046, 1000.000000000000000 ) ;
#15605 = CARTESIAN_POINT ( 'NONE',  ( -1.869504824896970119, -0.5046610169491535514, 5.548311746956866131 ) ) ;
#15606 = VECTOR ( 'NONE', #15537, 1000.000000000000000 ) ;
#15607 = EDGE_LOOP ( 'NONE', ( #15022, #12673, #2144, #1790 ) ) ;
#15608 = EDGE_CURVE ( 'NONE', #12725, #4752, #12411, .T. ) ;
#15609 = PLANE ( 'NONE',  #10527 ) ;
#15610 = CARTESIAN_POINT ( 'NONE',  ( -2.500000000000000000, 7.299999999999999822, 0.5999999999999999778 ) ) ;
#15611 = CARTESIAN_POINT ( 'NONE',  ( 1.000000000000000000, -5.500000000000000000, 5.100000000000000533 ) ) ;
#15612 = EDGE_CURVE ( 'NONE', #6456, #16165, #16052, .T. ) ;
#15613 = CARTESIAN_POINT ( 'NONE',  ( 1.181710496343130190, -2.798079561820010941, 6.378827610405712001 ) ) ;
#15614 = EDGE_CURVE ( 'NONE', #6904, #17710, #13354, .T. ) ;
#15615 = DIRECTION ( 'NONE',  ( -1.586032892321649771E-16, 0.000000000000000000, -1.000000000000000000 ) ) ;
#15616 = VECTOR ( 'NONE', #5875, 1000.000000000000000 ) ;
#15617 = ORIENTED_EDGE ( 'NONE', *, *, #13109, .F. ) ;
#15618 = DIRECTION ( 'NONE',  ( 1.216682766712499758E-16, 4.229421046191059358E-17, 1.000000000000000000 ) ) ;
#15619 = AXIS2_PLACEMENT_3D ( 'NONE', #3314, #4694, #1917 ) ;
#15620 = DIRECTION ( 'NONE',  ( 0.000000000000000000, 0.000000000000000000, -1.000000000000000000 ) ) ;
#15621 = ORIENTED_EDGE ( 'NONE', *, *, #12698, .T. ) ;
#15622 = VECTOR ( 'NONE', #12518, 1000.000000000000000 ) ;
#15623 = STYLED_ITEM ( 'NONE', ( #5839 ), #7724 ) ;
#15624 = LINE ( 'NONE', #1344, #10955 ) ;
#15625 = CARTESIAN_POINT ( 'NONE',  ( -1.965557623688110933, -5.511016949152534927, 5.292675575926340414 ) ) ;
#15626 = EDGE_LOOP ( 'NONE', ( #326, #5386, #3009, #17674 ) ) ;
#15627 = VECTOR ( 'NONE', #7980, 1000.000000000000000 ) ;
#15628 = CARTESIAN_POINT ( 'NONE',  ( 2.180207327701309428, -0.09343220338983103390, 5.586116916730190063 ) ) ;
#15629 = CARTESIAN_POINT ( 'NONE',  ( 1.641808337277750107, -5.413135593220339103, 6.386111670537619744 ) ) ;
#15630 = PLANE ( 'NONE',  #15299 ) ;
#15631 = ORIENTED_EDGE ( 'NONE', *, *, #7303, .F. ) ;
#15632 = CIRCLE ( 'NONE', #5263, 0.09999999999999986677 ) ;
#15633 = ADVANCED_FACE ( 'NONE', ( #3793 ), #2426, .F. ) ;
#15634 = DIRECTION ( 'NONE',  ( -1.000000000000000000, 0.000000000000000000, 0.000000000000000000 ) ) ;
#15635 = CARTESIAN_POINT ( 'NONE',  ( -2.313035575219740014, -1.427911429170980018, 5.134294963419759661 ) ) ;
#15636 = EDGE_CURVE ( 'NONE', #3897, #404, #15284, .T. ) ;
#15637 = LINE ( 'NONE', #2945, #14419 ) ;
#15638 = CARTESIAN_POINT ( 'NONE',  ( 1.124021676335459796, -2.010118636378181112, 2.982013645643220023 ) ) ;
#15639 =( GEOMETRIC_REPRESENTATION_CONTEXT ( 3 ) GLOBAL_UNCERTAINTY_ASSIGNED_CONTEXT ( ( #6949 ) ) GLOBAL_UNIT_ASSIGNED_CONTEXT ( ( #294, #10273, #1935 ) ) REPRESENTATION_CONTEXT ( 'NONE', 'WORKASPACE' ) );
#15640 = VECTOR ( 'NONE', #13340, 1000.000000000000000 ) ;
#15641 = CARTESIAN_POINT ( 'NONE',  ( 2.500000000000000000, 2.799999999999999822, 0.6099999999999999867 ) ) ;
#15642 = EDGE_LOOP ( 'NONE', ( #18104, #6401, #11848, #11040 ) ) ;
#15643 = CIRCLE ( 'NONE', #3487, 0.4000000000000000222 ) ;
#15644 = DIRECTION ( 'NONE',  ( -1.000000000000000000, 0.000000000000000000, 0.000000000000000000 ) ) ;
#15645 = CARTESIAN_POINT ( 'NONE',  ( 2.601107615185130673, -0.08453389830508521718, 5.226397344856369642 ) ) ;
#15646 = CARTESIAN_POINT ( 'NONE',  ( -2.334032080503389839, -3.310421904162350160, 5.001728246382240783 ) ) ;
#15647 = CARTESIAN_POINT ( 'NONE',  ( -0.4058874503045720172, 7.799999999999999822, 5.100000000000000533 ) ) ;
#15648 = CARTESIAN_POINT ( 'NONE',  ( 1.875000000000000000, 11.25000000000000000, 8.300000000000000711 ) ) ;
#15649 = CARTESIAN_POINT ( 'NONE',  ( -0.4221287159901280228, -5.157627118644064979, 7.320050063945812369 ) ) ;
#15650 = ORIENTED_EDGE ( 'NONE', *, *, #417, .T. ) ;
#15651 = ORIENTED_EDGE ( 'NONE', *, *, #1618, .T. ) ;
#15652 = LINE ( 'NONE', #8416, #14222 ) ;
#15653 = VECTOR ( 'NONE', #9553, 1000.000000000000000 ) ;
#15654 = VECTOR ( 'NONE', #13415, 1000.000000000000000 ) ;
#15655 = ORIENTED_EDGE ( 'NONE', *, *, #9596, .T. ) ;
#15656 = CARTESIAN_POINT ( 'NONE',  ( 2.510208264419000468, -1.074746228486680000, 5.561375738133185642 ) ) ;
#15657 = ADVANCED_FACE ( 'NONE', ( #6661 ), #7524, .F. ) ;
#15658 = VECTOR ( 'NONE', #15375, 1000.000000000000000 ) ;
#15659 = CARTESIAN_POINT ( 'NONE',  ( 0.009452110982655399438, -5.000192044704546035, 2.649999999999998579 ) ) ;
#15660 = CARTESIAN_POINT ( 'NONE',  ( 1.899999999999999911, 7.299999999999999822, 1.600000000000000089 ) ) ;
#15661 = CARTESIAN_POINT ( 'NONE',  ( 2.137408332595949645, -2.149848366107910191, 3.714996798363940034 ) ) ;
#15662 = DIRECTION ( 'NONE',  ( 1.000000000000000000, 0.000000000000000000, 0.000000000000000000 ) ) ;
#15663 = CARTESIAN_POINT ( 'NONE',  ( -0.2620510901103649815, -3.706322805063249959, 2.361180871966390260 ) ) ;
#15664 = VECTOR ( 'NONE', #13692, 1000.000000000000000 ) ;
#15665 = CARTESIAN_POINT ( 'NONE',  ( 1.750000000000000000, 0.5999999999999999778, 7.599999999999999645 ) ) ;
#15666 = CARTESIAN_POINT ( 'NONE',  ( 2.016543577558679079, -4.078935417675856101, 4.314702916654005627 ) ) ;
#15667 = DIRECTION ( 'NONE',  ( 1.000000000000000000, 2.220446049250309876E-16, -7.930164461608259947E-17 ) ) ;
#15668 = ORIENTED_EDGE ( 'NONE', *, *, #3121, .T. ) ;
#15669 = DIRECTION ( 'NONE',  ( -2.220446049250309876E-16, -1.000000000000000000, 0.000000000000000000 ) ) ;
#15670 = ORIENTED_EDGE ( 'NONE', *, *, #15065, .F. ) ;
#15671 = CARTESIAN_POINT ( 'NONE',  ( 1.800000000000000044, 11.29999999999999893, 1.600000000000000089 ) ) ;
#15672 = PLANE ( 'NONE',  #1022 ) ;
#15673 = ORIENTED_EDGE ( 'NONE', *, *, #14180, .T. ) ;
#15674 = DIRECTION ( 'NONE',  ( 1.306144734853129823E-16, -1.000000000000000000, 0.000000000000000000 ) ) ;
#15675 = ORIENTED_EDGE ( 'NONE', *, *, #13668, .F. ) ;
#15676 = CARTESIAN_POINT ( 'NONE',  ( 1.994315313497110997, -5.386440677966105817, 5.187224322759965922 ) ) ;
#15677 = CYLINDRICAL_SURFACE ( 'NONE', #10548, 0.6100000000000000977 ) ;
#15678 = DIRECTION ( 'NONE',  ( 0.000000000000000000, -1.000000000000000000, 0.000000000000000000 ) ) ;
#15679 = CARTESIAN_POINT ( 'NONE',  ( -1.899999999999999911, 10.00000000000000000, 1.600000000000000089 ) ) ;
#15680 = CARTESIAN_POINT ( 'NONE',  ( 1.899999999999999911, 11.40000000000000036, 7.550000000000000711 ) ) ;
#15681 = DIRECTION ( 'NONE',  ( 1.000000000000000000, 0.000000000000000000, 0.000000000000000000 ) ) ;
#15682 = DIRECTION ( 'NONE',  ( 1.000000000000000000, 0.000000000000000000, 0.000000000000000000 ) ) ;
#15683 = CARTESIAN_POINT ( 'NONE',  ( -1.236334101859210000, -2.029566048306499670, 2.697445712080720259 ) ) ;
#15684 = CARTESIAN_POINT ( 'NONE',  ( -0.1086361371090530797, -2.662190708450249854, 6.750146344128172160 ) ) ;
#15685 = DIRECTION ( 'NONE',  ( -6.123233995736779594E-17, -2.493473113004670213E-16, -1.000000000000000000 ) ) ;
#15686 = CIRCLE ( 'NONE', #10057, 0.4000000000000000222 ) ;
#15687 = CARTESIAN_POINT ( 'NONE',  ( -1.800000000000000044, 0.5999999999999999778, 6.599999999999999645 ) ) ;
#15688 = ORIENTED_EDGE ( 'NONE', *, *, #13566, .F. ) ;
#15689 = CARTESIAN_POINT ( 'NONE',  ( 1.392553072310509510, -0.03559322033898333626, 3.191531554476519261 ) ) ;
#15690 = CARTESIAN_POINT ( 'NONE',  ( -1.586727176531439909, -1.982989471729919906, 2.961885344765640138 ) ) ;
#15691 = ORIENTED_EDGE ( 'NONE', *, *, #4829, .F. ) ;
#15692 = VERTEX_POINT ( 'NONE', #5651 ) ;
#15693 = CARTESIAN_POINT ( 'NONE',  ( 2.255259958075439553, -3.896469987729530349, 5.372717034855999607 ) ) ;
#15694 = CARTESIAN_POINT ( 'NONE',  ( -2.268288188848061715, -5.551059322033894183, 3.322421079292323665 ) ) ;
#15695 = ORIENTED_EDGE ( 'NONE', *, *, #5692, .T. ) ;
#15696 = VECTOR ( 'NONE', #15807, 1000.000000000000000 ) ;
#15697 = CARTESIAN_POINT ( 'NONE',  ( -0.05465110135555984600, -0.4512711864406789841, 6.752241303418941243 ) ) ;
#15698 = ORIENTED_EDGE ( 'NONE', *, *, #12184, .T. ) ;
#15699 = LINE ( 'NONE', #3180, #4034 ) ;
#15700 = CARTESIAN_POINT ( 'NONE',  ( 1.399999999999999911, -9.500000000000000000, 3.299999999999999822 ) ) ;
#15701 = CARTESIAN_POINT ( 'NONE',  ( -1.238036348455400670, -2.006277760018210898, 3.062267469172299528 ) ) ;
#15702 = DIRECTION ( 'NONE',  ( -1.000000000000000000, 0.000000000000000000, 0.000000000000000000 ) ) ;
#15703 = CARTESIAN_POINT ( 'NONE',  ( 0.9664230948141925293, -0.3177966101694921219, 2.228384861502251457 ) ) ;
#15704 = ORIENTED_EDGE ( 'NONE', *, *, #6782, .T. ) ;
#15705 = LINE ( 'NONE', #14383, #6279 ) ;
#15706 = CARTESIAN_POINT ( 'NONE',  ( 1.500000000000000000, -5.599999999999999645, 2.299999999999999822 ) ) ;
#15707 = VERTEX_POINT ( 'NONE', #6853 ) ;
#15708 = VECTOR ( 'NONE', #12283, 1000.000000000000000 ) ;
#15709 = PLANE ( 'NONE',  #13308 ) ;
#15710 = CARTESIAN_POINT ( 'NONE',  ( -1.246151616534680651, -5.568855932203385706, 3.068501529594771071 ) ) ;
#15711 = EDGE_CURVE ( 'NONE', #1943, #1106, #6106, .T. ) ;
#15712 = CARTESIAN_POINT ( 'NONE',  ( -2.351526912647309953, -0.2269067796610170218, 4.606040641882809261 ) ) ;
#15713 = EDGE_CURVE ( 'NONE', #651, #11761, #94, .T. ) ;
#15714 = DIRECTION ( 'NONE',  ( 1.000000000000000000, 0.000000000000000000, 0.000000000000000000 ) ) ;
#15715 = EDGE_CURVE ( 'NONE', #1696, #14262, #15594, .T. ) ;
#15716 = ORIENTED_EDGE ( 'NONE', *, *, #15612, .T. ) ;
#15717 = DIRECTION ( 'NONE',  ( 5.421010862427519212E-16, 1.000000000000000000, 0.000000000000000000 ) ) ;
#15718 = CARTESIAN_POINT ( 'NONE',  ( 2.137408332595949645, -2.149848366107910191, 3.714996798363940034 ) ) ;
#15719 = CARTESIAN_POINT ( 'NONE',  ( -0.5999999999999999778, 0.5999999999999999778, 7.599999999999999645 ) ) ;
#15720 = VECTOR ( 'NONE', #12334, 1000.000000000000000 ) ;
#15721 = CARTESIAN_POINT ( 'NONE',  ( 1.698651900122530867, -2.406019537279079579, 5.853032334688926142 ) ) ;
#15722 = DIRECTION ( 'NONE',  ( -2.220446049250309876E-16, -1.000000000000000000, 0.000000000000000000 ) ) ;
#15723 = ORIENTED_EDGE ( 'NONE', *, *, #6311, .F. ) ;
#15724 = EDGE_CURVE ( 'NONE', #9388, #490, #9360, .T. ) ;
#15725 = DIRECTION ( 'NONE',  ( 1.000000000000000000, -2.220446049250310320E-15, 0.000000000000000000 ) ) ;
#15726 = CARTESIAN_POINT ( 'NONE',  ( 2.230812463554230352, -0.4023305084745772420, 6.137473736419911674 ) ) ;
#15727 = CARTESIAN_POINT ( 'NONE',  ( -2.352190863465239978, -4.917313796054239461, 4.622903765856379188 ) ) ;
#15728 = DIRECTION ( 'NONE',  ( 1.059965646700401283E-16, 0.6823182503600125903, 0.7310552682428677063 ) ) ;
#15729 = DIRECTION ( 'NONE',  ( -5.551115123125780730E-16, 0.000000000000000000, -1.000000000000000000 ) ) ;
#15730 = CARTESIAN_POINT ( 'NONE',  ( -2.614198783383141045, -5.233262711864406391, 4.243032045539295360 ) ) ;
#15731 = ORIENTED_EDGE ( 'NONE', *, *, #6169, .T. ) ;
#15732 = ADVANCED_FACE ( 'NONE', ( #2867 ), #11201, .T. ) ;
#15733 = EDGE_LOOP ( 'NONE', ( #7207, #13479, #16008, #17455 ) ) ;
#15734 = LINE ( 'NONE', #82, #16009 ) ;
#15735 = EDGE_CURVE ( 'NONE', #3530, #5195, #8517, .T. ) ;
#15736 = DIRECTION ( 'NONE',  ( -1.233581138472399909E-16, 1.000000000000000000, 1.233581138472399909E-16 ) ) ;
#15737 = ORIENTED_EDGE ( 'NONE', *, *, #13264, .F. ) ;
#15738 = CARTESIAN_POINT ( 'NONE',  ( -1.951437470830620136, -5.057043525783970317, 3.384463041838880137 ) ) ;
#15739 = CARTESIAN_POINT ( 'NONE',  ( 1.399999999999999911, 0.5999999999999999778, 6.100000000000000533 ) ) ;
#15740 = FACE_OUTER_BOUND ( 'NONE', #11674, .T. ) ;
#15741 = CARTESIAN_POINT ( 'NONE',  ( 0.09706517602699299418, -2.638902420161969520, 7.051451474958980725 ) ) ;
#15742 = CARTESIAN_POINT ( 'NONE',  ( 0.2570708662023959423, -5.304612347394245475, 2.048876625919409111 ) ) ;
#15743 = CARTESIAN_POINT ( 'NONE',  ( 2.313035575219750228, -4.172088570829020071, 5.134294963419709923 ) ) ;
#15744 = DIRECTION ( 'NONE',  ( 6.098637220230962441E-16, 1.000000000000000000, 0.000000000000000000 ) ) ;
#15745 = CARTESIAN_POINT ( 'NONE',  ( 0.5381211601353905749, -4.451548030288480895, 6.681243917250638376 ) ) ;
#15746 = CARTESIAN_POINT ( 'NONE',  ( 0.5999999999999999778, 0.5999999999999999778, 7.700000000000000178 ) ) ;
#15747 = FACE_OUTER_BOUND ( 'NONE', #15162, .T. ) ;
#15748 = VECTOR ( 'NONE', #12685, 1000.000000000000000 ) ;
#15749 = EDGE_LOOP ( 'NONE', ( #16223, #8880 ) ) ;
#15750 = EDGE_CURVE ( 'NONE', #6294, #16406, #1486, .T. ) ;
#15751 = DIRECTION ( 'NONE',  ( 0.000000000000000000, 0.000000000000000000, -1.000000000000000000 ) ) ;
#15752 = ORIENTED_EDGE ( 'NONE', *, *, #436, .T. ) ;
#15753 = PLANE ( 'NONE',  #11493 ) ;
#15754 = EDGE_LOOP ( 'NONE', ( #3173, #14055 ) ) ;
#15755 = CARTESIAN_POINT ( 'NONE',  ( -2.012177589105470066, -5.515466101694915579, 5.107213040360599088 ) ) ;
#15756 = CARTESIAN_POINT ( 'NONE',  ( 2.327043743583509627, -2.382731248990799244, 5.975923629552606364 ) ) ;
#15757 = SURFACE_STYLE_USAGE ( .BOTH. , #7585 ) ;
#15758 = LINE ( 'NONE', #3066, #4665 ) ;
#15759 = CARTESIAN_POINT ( 'NONE',  ( -1.864786684738369837, -4.804713230972779137, 2.817120744449669978 ) ) ;
#15760 = EDGE_CURVE ( 'NONE', #9237, #13339, #7308, .T. ) ;
#15761 = DIRECTION ( 'NONE',  ( -4.498716214366520783E-15, 1.000000000000000000, 7.401486830834380223E-16 ) ) ;
#15762 = DIRECTION ( 'NONE',  ( -1.000000000000000000, 0.000000000000000000, 0.000000000000000000 ) ) ;
#15763 = CARTESIAN_POINT ( 'NONE',  ( -1.948278411993560111, -3.193980462720909852, 6.020210936496040333 ) ) ;
#15764 = CARTESIAN_POINT ( 'NONE',  ( 1.616473591439308688, -3.989623140882693875, 5.965667796385536903 ) ) ;
#15765 = DIRECTION ( 'NONE',  ( 1.110223024625159992E-16, 0.000000000000000000, -1.000000000000000000 ) ) ;
#15766 = DIRECTION ( 'NONE',  ( 0.000000000000000000, 0.000000000000000000, -1.000000000000000000 ) ) ;
#15767 = ORIENTED_EDGE ( 'NONE', *, *, #13683, .T. ) ;
#15768 = CARTESIAN_POINT ( 'NONE',  ( -0.5134687485629449988, -3.384127645387192018, 2.096259702418250104 ) ) ;
#15769 = EDGE_CURVE ( 'NONE', #16005, #13449, #12499, .T. ) ;
#15770 = CARTESIAN_POINT ( 'NONE',  ( -1.949083719010310078, -0.2402542372881359412, 4.055210292801460170 ) ) ;
#15771 = CARTESIAN_POINT ( 'NONE',  ( 1.444955263746720009, -2.332313796054249710, 2.842353646881480511 ) ) ;
#15772 = VERTEX_POINT ( 'NONE', #10090 ) ;
#15773 = CARTESIAN_POINT ( 'NONE',  ( 1.899999999999999911, 11.40000000000000036, 6.599999999999999645 ) ) ;
#15774 = ORIENTED_EDGE ( 'NONE', *, *, #6663, .F. ) ;
#15775 = CARTESIAN_POINT ( 'NONE',  ( 1.710920205120059823, -4.012911429170970656, 6.316012914303540171 ) ) ;
#15776 = APPLICATION_PROTOCOL_DEFINITION ( 'draft international standard', 'automotive_design', 1998, #4584 ) ;
#15777 = CARTESIAN_POINT ( 'NONE',  ( 2.416676968769261080, -5.095338983050850423, 5.796598111919825769 ) ) ;
#15778 = ORIENTED_EDGE ( 'NONE', *, *, #11534, .T. ) ;
#15779 = CARTESIAN_POINT ( 'NONE',  ( 0.8570167067220200163, -0.3177966101694920664, 2.508190348879349774 ) ) ;
#15780 = VERTEX_POINT ( 'NONE', #174 ) ;
#15781 = DIRECTION ( 'NONE',  ( 0.000000000000000000, 1.421904488505579605E-15, -1.000000000000000000 ) ) ;
#15782 = CARTESIAN_POINT ( 'NONE',  ( -0.5999999999999999778, 0.5999999999999999778, 7.700000000000000178 ) ) ;
#15783 = LINE ( 'NONE', #3092, #5594 ) ;
#15784 = CARTESIAN_POINT ( 'NONE',  ( -1.313542260532420292, -3.124115597856051085, 6.277817661335885369 ) ) ;
#15785 = CARTESIAN_POINT ( 'NONE',  ( 1.255262969126039558E-16, -0.3000000000000002665, 2.050000000000001155 ) ) ;
#15786 = ORIENTED_EDGE ( 'NONE', *, *, #4708, .T. ) ;
#15787 = VECTOR ( 'NONE', #1585, 1000.000000000000000 ) ;
#15788 = DIRECTION ( 'NONE',  ( -2.537652627714639929E-16, -1.000000000000000000, 0.000000000000000000 ) ) ;
#15789 = EDGE_LOOP ( 'NONE', ( #4775, #6099, #13124, #15417 ) ) ;
#15790 = CARTESIAN_POINT ( 'NONE',  ( 1.399999999999999911, 0.5999999999999999778, 6.100000000000000533 ) ) ;
#15791 = CARTESIAN_POINT ( 'NONE',  ( 1.713314936023349944, -5.338983050847460277, 3.089913064446569546 ) ) ;
#15792 = FILL_AREA_STYLE_COLOUR ( '', #18265 ) ;
#15793 = CARTESIAN_POINT ( 'NONE',  ( -0.9193620247240871235, -0.2831443699174389095, 2.206709149717571261 ) ) ;
#15794 = EDGE_CURVE ( 'NONE', #4541, #13931, #14682, .T. ) ;
#15795 = CARTESIAN_POINT ( 'NONE',  ( -3.408368997776849933E-15, -5.599999999999999645, 2.350000000000000089 ) ) ;
#15796 = CARTESIAN_POINT ( 'NONE',  ( -0.6096110657044609971, -1.800524041783589935, 2.426869991387519576 ) ) ;
#15797 = LINE ( 'NONE', #502, #3774 ) ;
#15798 = CARTESIAN_POINT ( 'NONE',  ( -1.736825397686170502, -1.614217735477279536, 3.605313112995154334 ) ) ;
#15799 = FACE_OUTER_BOUND ( 'NONE', #11302, .T. ) ;
#15800 = EDGE_LOOP ( 'NONE', ( #16288, #11389, #16878, #10971 ) ) ;
#15801 = EDGE_CURVE ( 'NONE', #9351, #6214, #11382, .T. ) ;
#15802 = LINE ( 'NONE', #4571, #11192 ) ;
#15803 = VECTOR ( 'NONE', #2513, 1000.000000000000000 ) ;
#15804 = CARTESIAN_POINT ( 'NONE',  ( 0.2469343877495150108, -0.004449152542373164231, 2.057675570509529539 ) ) ;
#15805 = CARTESIAN_POINT ( 'NONE',  ( 1.026235786675480099, -4.404971453711899798, 6.817920158464540137 ) ) ;
#15806 = CARTESIAN_POINT ( 'NONE',  ( 0.1749999999999999889, 9.099999999999999645, 0.5999999999999999778 ) ) ;
#15807 = DIRECTION ( 'NONE',  ( 0.000000000000000000, 0.000000000000000000, 1.000000000000000000 ) ) ;
#15808 = CARTESIAN_POINT ( 'NONE',  ( -3.188875856275119715E-15, -5.300000000000000711, 2.050000000000001155 ) ) ;
#15809 = VERTEX_POINT ( 'NONE', #18113 ) ;
#15810 = ORIENTED_EDGE ( 'NONE', *, *, #10008, .F. ) ;
#15811 = DIRECTION ( 'NONE',  ( -2.220446049250309876E-16, -1.000000000000000000, -4.930380657631319405E-32 ) ) ;
#15812 =( NAMED_UNIT ( * ) SI_UNIT ( $, .STERADIAN. ) SOLID_ANGLE_UNIT ( ) );
#15813 = CARTESIAN_POINT ( 'NONE',  ( -0.8740908734716290596, 4.154758922476410099, 8.300000000000000711 ) ) ;
#15814 = ORIENTED_EDGE ( 'NONE', *, *, #15317, .T. ) ;
#15815 = EDGE_CURVE ( 'NONE', #9659, #7174, #4332, .T. ) ;
#15816 = CARTESIAN_POINT ( 'NONE',  ( 1.923406176634910203, -0.8030495317899833951, 2.875176962145290727 ) ) ;
#15817 = ADVANCED_FACE ( 'NONE', ( #11101 ), #16846, .T. ) ;
#15818 = CARTESIAN_POINT ( 'NONE',  ( -1.250000000000000000, 5.012741699796949391, 5.100000000000000533 ) ) ;
#15819 = LINE ( 'NONE', #3388, #4339 ) ;
#15820 = CARTESIAN_POINT ( 'NONE',  ( 1.507201387236020151, -2.475884402143949892, 6.507509243627189299 ) ) ;
#15821 = EDGE_CURVE ( 'NONE', #11761, #8948, #9997, .T. ) ;
#15822 = ADVANCED_FACE ( 'NONE', ( #8612 ), #8339, .F. ) ;
#15823 = CARTESIAN_POINT ( 'NONE',  ( 0.2270348434643680025, -5.304612347394249916, 2.348896311281980065 ) ) ;
#15824 = CARTESIAN_POINT ( 'NONE',  ( -2.296954468777729463, -4.963890372630819670, 4.187412587068699565 ) ) ;
#15825 = ADVANCED_FACE ( 'NONE', ( #14255 ), #9, .F. ) ;
#15826 = DIRECTION ( 'NONE',  ( 0.7071067811865480168, 0.000000000000000000, 0.7071067811865470176 ) ) ;
#15827 = EDGE_CURVE ( 'NONE', #13928, #17154, #15560, .T. ) ;
#15828 = CARTESIAN_POINT ( 'NONE',  ( -1.802718065953990978, -5.033755237495684653, 3.717600174934233781 ) ) ;
#15829 = DIRECTION ( 'NONE',  ( 1.850371707708589879E-16, 1.000000000000000000, 0.000000000000000000 ) ) ;
#15830 = EDGE_CURVE ( 'NONE', #7556, #7904, #13134, .T. ) ;
#15831 = VECTOR ( 'NONE', #3549, 1000.000000000000000 ) ;
#15832 = CARTESIAN_POINT ( 'NONE',  ( -0.2812789908084309953, -0.4557203389830509765, 7.036533610117280624 ) ) ;
#15833 = DIRECTION ( 'NONE',  ( 6.123233995736768501E-17, 0.000000000000000000, 1.000000000000000000 ) ) ;
#15834 = ORIENTED_EDGE ( 'NONE', *, *, #2350, .T. ) ;
#15835 = SURFACE_STYLE_USAGE ( .BOTH. , #12790 ) ;
#15836 = ORIENTED_EDGE ( 'NONE', *, *, #1328, .F. ) ;
#15837 = DIRECTION ( 'NONE',  ( -1.908195823574489776E-16, 1.000000000000000000, 0.000000000000000000 ) ) ;
#15838 = CARTESIAN_POINT ( 'NONE',  ( 0.1749999999999999889, 5.200000000000000178, 0.5999999999999999778 ) ) ;
#15839 = EDGE_LOOP ( 'NONE', ( #8967, #14067, #7414, #3909, #17611, #4190, #4519, #14657, #1851, #509, #2259, #16788, #9400, #2910, #6080, #12330, #2362, #8951, #4811, #5489, #11483, #17747, #11258, #6578, #13513, #15786 ) ) ;
#15840 = CARTESIAN_POINT ( 'NONE',  ( 1.494593880360790550, -5.338983050847455836, 3.295456077495951153 ) ) ;
#15841 = CARTESIAN_POINT ( 'NONE',  ( -1.889999999999999902, 4.700000000000000178, 0.5999999999999999778 ) ) ;
#15842 = CARTESIAN_POINT ( 'NONE',  ( 1.292937800126339631, -2.522460978720530989, 7.017633607369027082 ) ) ;
#15843 = CARTESIAN_POINT ( 'NONE',  ( -1.899999999999999911, 0.5999999999999999778, 0.5999999999999999778 ) ) ;
#15844 = DIRECTION ( 'NONE',  ( 0.000000000000000000, 0.000000000000000000, -1.000000000000000000 ) ) ;
#15845 = EDGE_CURVE ( 'NONE', #396, #9909, #5917, .T. ) ;
#15846 = LINE ( 'NONE', #4619, #8818 ) ;
#15847 = CARTESIAN_POINT ( 'NONE',  ( -0.5500000000000000444, 6.450000000000000178, 3.200000000000000178 ) ) ;
#15848 = CARTESIAN_POINT ( 'NONE',  ( -1.145304265383870090, -3.077539021279469988, 6.755972720436099088 ) ) ;
#15849 = CARTESIAN_POINT ( 'NONE',  ( -0.05638445020225820586, -4.222506023765566496, 6.752248190741917178 ) ) ;
#15850 = DIRECTION ( 'NONE',  ( 4.440892098500620245E-16, -3.700743415417219694E-16, 1.000000000000000000 ) ) ;
#15851 = DIRECTION ( 'NONE',  ( 0.000000000000000000, -1.000000000000000000, 0.000000000000000000 ) ) ;
#15852 = ORIENTED_EDGE ( 'NONE', *, *, #1271, .F. ) ;
#15853 = CARTESIAN_POINT ( 'NONE',  ( -1.032615103526609568, -4.315659176918716255, 7.144753513336388195 ) ) ;
#15854 = CARTESIAN_POINT ( 'NONE',  ( -1.134881315981510541, -0.1779661016949160846, 6.410767520434657918 ) ) ;
#15855 = CARTESIAN_POINT ( 'NONE',  ( 1.167621112247380077, -2.821367850108300157, 6.743381174846749815 ) ) ;
#15856 = ORIENTED_EDGE ( 'NONE', *, *, #8575, .F. ) ;
#15857 = DIRECTION ( 'NONE',  ( 9.349246523159210481E-16, 0.000000000000000000, 1.000000000000000000 ) ) ;
#15858 = ORIENTED_EDGE ( 'NONE', *, *, #11733, .F. ) ;
#15859 = AXIS2_PLACEMENT_3D ( 'NONE', #16468, #2499, #9617 ) ;
#15860 = CARTESIAN_POINT ( 'NONE',  ( -0.8748826269293140667, -3.337551068810609145, 2.515205712983220820 ) ) ;
#15861 = CARTESIAN_POINT ( 'NONE',  ( 2.586172839791708533, -5.064194915254235596, 4.104546363490936045 ) ) ;
#15862 = CARTESIAN_POINT ( 'NONE',  ( 2.350000000000000089, -5.599999999999999645, 2.799999999999999822 ) ) ;
#15863 = AXIS2_PLACEMENT_3D ( 'NONE', #15473, #17110, #18201 ) ;
#15864 = ORIENTED_EDGE ( 'NONE', *, *, #17826, .F. ) ;
#15865 = AXIS2_PLACEMENT_3D ( 'NONE', #13597, #16272, #10715 ) ;
#15866 = DIRECTION ( 'NONE',  ( 1.000000000000000000, -1.224646799147350002E-16, 0.000000000000000000 ) ) ;
#15867 = CARTESIAN_POINT ( 'NONE',  ( 1.800000000000000044, 0.5999999999999999778, 6.599999999999999645 ) ) ;
#15868 = ORIENTED_EDGE ( 'NONE', *, *, #12439, .T. ) ;
#15869 = ADVANCED_FACE ( 'NONE', ( #3048 ), #4591, .F. ) ;
#15870 = CARTESIAN_POINT ( 'NONE',  ( 1.899999999999999911, 0.5999999999999999778, 7.550000000000000711 ) ) ;
#15871 = CARTESIAN_POINT ( 'NONE',  ( -2.035869680587120811, -3.310421904162345719, 4.964832940349540813 ) ) ;
#15872 = DIRECTION ( 'NONE',  ( 2.220446049250309876E-16, -1.110223024625159992E-16, -1.000000000000000000 ) ) ;
#15873 = CARTESIAN_POINT ( 'NONE',  ( 2.540842781840729536, -0.3889830508474575455, 5.466141598148674952 ) ) ;
#15874 = ORIENTED_EDGE ( 'NONE', *, *, #3688, .T. ) ;
#15875 = DIRECTION ( 'NONE',  ( 0.7071067811865470176, -0.7071067811865480168, 0.000000000000000000 ) ) ;
#15876 = AXIS2_PLACEMENT_3D ( 'NONE', #11882, #3887, #13791 ) ;
#15877 = ORIENTED_EDGE ( 'NONE', *, *, #14101, .F. ) ;
#15878 = AXIS2_PLACEMENT_3D ( 'NONE', #1929, #7768, #6097 ) ;
#15879 = DIRECTION ( 'NONE',  ( 6.167905692361979821E-17, 0.000000000000000000, 1.000000000000000000 ) ) ;
#15880 = CARTESIAN_POINT ( 'NONE',  ( -2.022304719220918479, -5.533262711864405325, 4.346496488058700258 ) ) ;
#15881 = CARTESIAN_POINT ( 'NONE',  ( -2.155845792290839391, -0.2447033898305089883, 3.756158857535781159 ) ) ;
#15882 = AXIS2_PLACEMENT_3D ( 'NONE', #755, #12059, #9465 ) ;
#15883 = AXIS2_PLACEMENT_3D ( 'NONE', #7195, #1633, #5624 ) ;
#15884 = CARTESIAN_POINT ( 'NONE',  ( 1.152986057739970205, -3.846052534792983923, 2.309657588616410351 ) ) ;
#15885 = ORIENTED_EDGE ( 'NONE', *, *, #11964, .T. ) ;
#15886 = CARTESIAN_POINT ( 'NONE',  ( -1.764807890102220167, -3.221109627369169726, 3.143016121304770039 ) ) ;
#15887 = VECTOR ( 'NONE', #16366, 1000.000000000000000 ) ;
#15888 = CARTESIAN_POINT ( 'NONE',  ( 0.5000000000000000000, 5.762741699796949391, 6.100000000000000533 ) ) ;
#15889 = COLOUR_RGB ( '', 0.31764706, 0.68627451, 0.89019608) ;
#15890 = CARTESIAN_POINT ( 'NONE',  ( -0.7128755192781907057, -1.777235753495299608, 2.774718115017459130 ) ) ;
#15891 = AXIS2_PLACEMENT_3D ( 'NONE', #3879, #2316, #9532 ) ;
#15892 = DIRECTION ( 'NONE',  ( 6.123233995736767268E-17, 0.000000000000000000, 1.000000000000000000 ) ) ;
#15893 = LINE ( 'NONE', #3205, #18279 ) ;
#15894 = ORIENTED_EDGE ( 'NONE', *, *, #17723, .F. ) ;
#15895 = CIRCLE ( 'NONE', #7908, 0.5999999999999998668 ) ;
#15896 = AXIS2_PLACEMENT_3D ( 'NONE', #11961, #14479, #402 ) ;
#15897 = CIRCLE ( 'NONE', #15019, 0.4166666666666671848 ) ;
#15898 = CARTESIAN_POINT ( 'NONE',  ( 1.850000000000000089, 0.7500000000000000000, 7.700000000000000178 ) ) ;
#15899 = CARTESIAN_POINT ( 'NONE',  ( 0.04351999560419626129, -1.078587104846650213, 7.353529668759038351 ) ) ;
#15900 = CARTESIAN_POINT ( 'NONE',  ( 1.994983296312400123, -4.265241723982169830, 5.948514050749290405 ) ) ;
#15901 = DIRECTION ( 'NONE',  ( 0.000000000000000000, -1.000000000000000000, 0.000000000000000000 ) ) ;
#15902 = DIRECTION ( 'NONE',  ( 0.000000000000000000, -1.000000000000000000, 0.000000000000000000 ) ) ;
#15903 = CARTESIAN_POINT ( 'NONE',  ( 1.031876288691629506, -5.130932203389829915, 7.145012538880298081 ) ) ;
#15904 = ORIENTED_EDGE ( 'NONE', *, *, #12230, .F. ) ;
#15905 = VECTOR ( 'NONE', #6159, 1000.000000000000000 ) ;
#15906 = AXIS2_PLACEMENT_3D ( 'NONE', #3484, #4969, #624 ) ;
#15907 = ORIENTED_EDGE ( 'NONE', *, *, #2272, .F. ) ;
#15908 = DIRECTION ( 'NONE',  ( 4.318427418585891014E-15, -2.220446049250315053E-16, 1.000000000000000000 ) ) ;
#15909 = PLANE ( 'NONE',  #15005 ) ;
#15910 = EDGE_LOOP ( 'NONE', ( #4144, #9418, #553, #4880 ) ) ;
#15911 = CARTESIAN_POINT ( 'NONE',  ( -2.380466601827099016, -1.889836318576769036, 3.526759849567179916 ) ) ;
#15912 = AXIS2_PLACEMENT_3D ( 'NONE', #2976, #9908, #15564 ) ;
#15913 = CARTESIAN_POINT ( 'NONE',  ( 0.9930264841371569950, -0.4076464065212260235, 2.562902636367419884 ) ) ;
#15914 = LINE ( 'NONE', #7215, #15596 ) ;
#15915 = CARTESIAN_POINT ( 'NONE',  ( 0.8986180677147459495, -1.963542059801610229, 2.524860635301609868 ) ) ;
#15916 = CARTESIAN_POINT ( 'NONE',  ( 1.484081582636959551, -5.328211948015596278, 2.487334927317659705 ) ) ;
#15917 = CIRCLE ( 'NONE', #6138, 0.2500000000000002220 ) ;
#15918 = CARTESIAN_POINT ( 'NONE',  ( -2.091881088960070745, -1.610376859117309767, 6.333140288723886790 ) ) ;
#15919 = VECTOR ( 'NONE', #1508, 1000.000000000000000 ) ;
#15920 = DIRECTION ( 'NONE',  ( -1.000000000000000000, 0.000000000000000000, 2.220446049250319983E-16 ) ) ;
#15921 = CARTESIAN_POINT ( 'NONE',  ( -2.028464043723881005, -4.870737219477664581, 5.016599851465114668 ) ) ;
#15922 = CYLINDRICAL_SURFACE ( 'NONE', #17041, 0.6100000000000000977 ) ;
#15923 = VECTOR ( 'NONE', #11452, 1000.000000000000000 ) ;
#15924 = CARTESIAN_POINT ( 'NONE',  ( 2.340070819011249803, -0.3800847457627120063, 4.950151441910540129 ) ) ;
#15925 = VECTOR ( 'NONE', #12257, 1000.000000000000000 ) ;
#15926 = CARTESIAN_POINT ( 'NONE',  ( -0.5999999999999999778, 0.5999999999999999778, 7.599999999999999645 ) ) ;
#15927 = EDGE_LOOP ( 'NONE', ( #2981, #876, #4070, #11913 ) ) ;
#15928 = LINE ( 'NONE', #3236, #8121 ) ;
#15929 = EDGE_LOOP ( 'NONE', ( #5726, #15716, #18193, #17784 ) ) ;
#15930 = FACE_OUTER_BOUND ( 'NONE', #6389, .T. ) ;
#15931 = LINE ( 'NONE', #7860, #5287 ) ;
#15932 = PRODUCT_DEFINITION ( 'UNKNOWN', '', #17414, #17859 ) ;
#15933 = EDGE_CURVE ( 'NONE', #16352, #6699, #6184, .T. ) ;
#15934 = AXIS2_PLACEMENT_3D ( 'NONE', #2814, #8556, #14202 ) ;
#15935 = ORIENTED_EDGE ( 'NONE', *, *, #11843, .T. ) ;
#15936 = ADVANCED_FACE ( 'NONE', ( #7403 ), #13387, .T. ) ;
#15937 = CARTESIAN_POINT ( 'NONE',  ( -1.042222075699109407, -5.475423728813556323, 6.468743694056166227 ) ) ;
#15938 = EDGE_CURVE ( 'NONE', #16796, #13279, #17634, .T. ) ;
#15939 = CARTESIAN_POINT ( 'NONE',  ( 0.5372984490435490645, 4.599999999999999645, 7.700000000000000178 ) ) ;
#15940 = CARTESIAN_POINT ( 'NONE',  ( -1.381042549632419902, -1.540511994252449890, 6.605640880016140137 ) ) ;
#15941 = CARTESIAN_POINT ( 'NONE',  ( -1.315254646989760134, -2.778632149891700376, 7.005042061779727547 ) ) ;
#15942 =( LENGTH_UNIT ( ) NAMED_UNIT ( * ) SI_UNIT ( .MILLI., .METRE. ) );
#15943 = FILL_AREA_STYLE ('',( #295 ) ) ;
#15944 = CIRCLE ( 'NONE', #4113, 0.09999999999999997780 ) ;
#15945 = CARTESIAN_POINT ( 'NONE',  ( -1.149999999999999911, 9.299999999999998934, 7.500000000000000000 ) ) ;
#15946 = AXIS2_PLACEMENT_3D ( 'NONE', #15847, #15948, #15762 ) ;
#15947 = CARTESIAN_POINT ( 'NONE',  ( -1.381042549632419902, -1.540511994252449890, 6.605640880016140137 ) ) ;
#15948 = DIRECTION ( 'NONE',  ( -1.224646799147350002E-16, 1.000000000000000000, 6.123233995736769734E-17 ) ) ;
#15949 = CARTESIAN_POINT ( 'NONE',  ( -2.218077401483159683, -4.824160642901089702, 5.486688202856539576 ) ) ;
#15950 = CARTESIAN_POINT ( 'NONE',  ( -2.033547680391670998, -4.641695212954759064, 4.417890669792460479 ) ) ;
#15951 = AXIS2_PLACEMENT_3D ( 'NONE', #8417, #15024, #9894 ) ;
#15952 = CARTESIAN_POINT ( 'NONE',  ( 0.009417288784632644669, -5.000743947056720096, 2.370019840861731897 ) ) ;
#15953 = CARTESIAN_POINT ( 'NONE',  ( 1.850000000000000089, 11.25000000000000000, 8.300000000000000711 ) ) ;
#15954 = ORIENTED_EDGE ( 'NONE', *, *, #17063, .F. ) ;
#15955 = ADVANCED_FACE ( 'NONE', ( #14889 ), #15305, .T. ) ;
#15956 = CARTESIAN_POINT ( 'NONE',  ( 1.351903350398191206, -0.1156779661016950206, 6.245004350000406212 ) ) ;
#15957 = CARTESIAN_POINT ( 'NONE',  ( 0.5570002967656469961, -2.891232714973159812, 6.986590552960210587 ) ) ;
#15958 = VERTEX_POINT ( 'NONE', #5066 ) ;
#15959 = AXIS2_PLACEMENT_3D ( 'NONE', #10803, #13395, #3861 ) ;
#15960 = ORIENTED_EDGE ( 'NONE', *, *, #4045, .T. ) ;
#15961 = DIRECTION ( 'NONE',  ( 6.123233995736767268E-17, -1.000000000000000000, 0.000000000000000000 ) ) ;
#15962 = ADVANCED_FACE ( 'NONE', ( #10808 ), #6637, .T. ) ;
#15963 = EDGE_LOOP ( 'NONE', ( #1693, #15767, #13296, #4788 ) ) ;
#15964 = CARTESIAN_POINT ( 'NONE',  ( -1.794646911016549495, -4.432100618360158784, 6.222494056560700315 ) ) ;
#15965 = CARTESIAN_POINT ( 'NONE',  ( 0.000000000000000000, 0.000000000000000000, 0.000000000000000000 ) ) ;
#15966 = CARTESIAN_POINT ( 'NONE',  ( -0.4917262214559124933, -5.591101694915256104, 2.092115739186370948 ) ) ;
#15967 = ORIENTED_EDGE ( 'NONE', *, *, #3031, .F. ) ;
#15968 = CARTESIAN_POINT ( 'NONE',  ( -1.250000000000000000, 7.799999999999999822, 5.100000000000000533 ) ) ;
#15969 = CARTESIAN_POINT ( 'NONE',  ( -2.143090896833110381, -0.5046610169491529962, 5.672454929438350391 ) ) ;
#15970 = ORIENTED_EDGE ( 'NONE', *, *, #9354, .T. ) ;
#15971 = DIRECTION ( 'NONE',  ( 2.220446049250309876E-16, 0.000000000000000000, -1.000000000000000000 ) ) ;
#15972 = AXIS2_PLACEMENT_3D ( 'NONE', #14243, #18102, #14149 ) ;
#15973 = CARTESIAN_POINT ( 'NONE',  ( 1.741179788930650840, -4.265241723982168942, 5.787747574231955738 ) ) ;
#15974 = CARTESIAN_POINT ( 'NONE',  ( -1.254903241568450900, -0.4735169491525429986, 7.038391080368498365 ) ) ;
#15975 = ORIENTED_EDGE ( 'NONE', *, *, #3144, .F. ) ;
#15976 = DIRECTION ( 'NONE',  ( -1.000000000000000000, 0.000000000000000000, 1.142385477618690234E-14 ) ) ;
#15977 = ORIENTED_EDGE ( 'NONE', *, *, #8461, .T. ) ;
#15978 = CARTESIAN_POINT ( 'NONE',  ( 0.0003104168811371160069, -0.4450801552861859967, 2.198280450787269746 ) ) ;
#15979 = CARTESIAN_POINT ( 'NONE',  ( -0.5889081234606770021, -5.462076271186440124, 6.978529000034869867 ) ) ;
#15980 = APPLICATION_CONTEXT ( 'automotive_design' ) ;
#15981 = EDGE_CURVE ( 'NONE', #4246, #6244, #492, .T. ) ;
#15982 = CARTESIAN_POINT ( 'NONE',  ( -2.350067830300900162, -0.2224576271186440024, 4.825253242917700192 ) ) ;
#15983 = AXIS2_PLACEMENT_3D ( 'NONE', #14873, #3562, #6431 ) ;
#15984 = CARTESIAN_POINT ( 'NONE',  ( 2.107551805806971323, -4.288530012270460823, 6.312866726931170902 ) ) ;
#15985 = EDGE_LOOP ( 'NONE', ( #1417, #14765, #47, #984 ) ) ;
#15986 = CARTESIAN_POINT ( 'NONE',  ( 2.062913653388430024, -2.382731248990799688, 5.832754583370790336 ) ) ;
#15987 = DIRECTION ( 'NONE',  ( 0.000000000000000000, 1.000000000000000000, 2.775557561562890365E-16 ) ) ;
#15988 = DIRECTION ( 'NONE',  ( 0.000000000000000000, 0.000000000000000000, 1.000000000000000000 ) ) ;
#15989 = CARTESIAN_POINT ( 'NONE',  ( 1.454969160282001406, -2.452596113855660676, 6.148435909958180901 ) ) ;
#15990 = CARTESIAN_POINT ( 'NONE',  ( -0.7999999999998790301, 11.40000000000000036, -9.797174393178840942E-17 ) ) ;
#15991 = CYLINDRICAL_SURFACE ( 'NONE', #11802, 0.1999999999999996503 ) ;
#15992 = ORIENTED_EDGE ( 'NONE', *, *, #11553, .T. ) ;
#15993 = VECTOR ( 'NONE', #7294, 1000.000000000000000 ) ;
#15994 = LINE ( 'NONE', #3298, #15923 ) ;
#15995 = EDGE_CURVE ( 'NONE', #475, #8344, #7846, .T. ) ;
#15996 = CARTESIAN_POINT ( 'NONE',  ( 2.293791554891360551, -0.8224159336754829353, 6.034778631725497000 ) ) ;
#15997 = ORIENTED_EDGE ( 'NONE', *, *, #2918, .T. ) ;
#15998 = CARTESIAN_POINT ( 'NONE',  ( -0.4735094604798580353, -4.567989471729919870, 7.005327412390699671 ) ) ;
#15999 = DIRECTION ( 'NONE',  ( 0.000000000000000000, 0.000000000000000000, -1.000000000000000000 ) ) ;
#16000 = CARTESIAN_POINT ( 'NONE',  ( 0.6207106781186539912, 6.450000000000000178, 2.628553390593269423 ) ) ;
#16001 = CARTESIAN_POINT ( 'NONE',  ( -1.554165089654128584, -5.179872881355935377, 6.851145244874527584 ) ) ;
#16002 = ORIENTED_EDGE ( 'NONE', *, *, #3937, .T. ) ;
#16003 = EDGE_CURVE ( 'NONE', #2052, #15500, #13496, .T. ) ;
#16004 = SHAPE_REPRESENTATION ( 'Actuator Spring Stop Clip', ( #17681 ), #5599 ) ;
#16005 = VERTEX_POINT ( 'NONE', #2403 ) ;
#16006 = DIRECTION ( 'NONE',  ( -2.168404344971009262E-15, -1.000000000000000000, -2.220446049250220143E-16 ) ) ;
#16007 = PLANE ( 'NONE',  #10249 ) ;
#16008 = ORIENTED_EDGE ( 'NONE', *, *, #9405, .T. ) ;
#16009 = VECTOR ( 'NONE', #12851, 1000.000000000000000 ) ;
#16010 = DIRECTION ( 'NONE',  ( 2.960594732333750117E-16, 1.000000000000000000, 0.000000000000000000 ) ) ;
#16011 = CARTESIAN_POINT ( 'NONE',  ( -1.392767620582729293, -2.029566048306499670, 2.440948861123721780 ) ) ;
#16012 = DIRECTION ( 'NONE',  ( 9.349246523159200620E-16, 0.000000000000000000, -1.000000000000000000 ) ) ;
#16013 = DIRECTION ( 'NONE',  ( -1.480297366166879989E-16, 0.000000000000000000, 1.000000000000000000 ) ) ;
#16014 = CARTESIAN_POINT ( 'NONE',  ( -1.962536940652960027, -2.895073591333140239, 5.998920491814800471 ) ) ;
#16015 = CARTESIAN_POINT ( 'NONE',  ( 1.319613955262860072, -5.028306595106929677, 2.740497729816110173 ) ) ;
#16016 = CARTESIAN_POINT ( 'NONE',  ( 2.651429253058529945, -0.9815930753335269099, 4.585822029124893895 ) ) ;
#16017 = CYLINDRICAL_SURFACE ( 'NONE', #2752, 0.01000000000000002623 ) ;
#16018 = CARTESIAN_POINT ( 'NONE',  ( -0.5972539422561604638, -4.591277760018214416, 6.664227474374482263 ) ) ;
#16019 = EDGE_CURVE ( 'NONE', #6826, #5242, #13208, .T. ) ;
#16020 = CARTESIAN_POINT ( 'NONE',  ( -1.899999999999999911, 11.25000000000000000, 7.649999999999999467 ) ) ;
#16021 = VERTEX_POINT ( 'NONE', #12390 ) ;
#16022 = CARTESIAN_POINT ( 'NONE',  ( -1.192893218813449785, -10.00000000000000000, 3.507106781186551725 ) ) ;
#16023 = ORIENTED_EDGE ( 'NONE', *, *, #6779, .F. ) ;
#16024 = CARTESIAN_POINT ( 'NONE',  ( 0.5500000000000000444, 6.450000000000000178, 3.600000000000000089 ) ) ;
#16025 = DIRECTION ( 'NONE',  ( 1.000000000000000000, 0.000000000000000000, 0.000000000000000000 ) ) ;
#16026 = ORIENTED_EDGE ( 'NONE', *, *, #11332, .F. ) ;
#16027 = CARTESIAN_POINT ( 'NONE',  ( -1.044181395669830259, -2.052854336594790219, 2.590869634085910089 ) ) ;
#16028 =( NAMED_UNIT ( * ) PLANE_ANGLE_UNIT ( ) SI_UNIT ( $, .RADIAN. ) );
#16029 = CARTESIAN_POINT ( 'NONE',  ( 2.328217775191430139, -5.381991525423729605, 5.043379051721160522 ) ) ;
#16030 = DIRECTION ( 'NONE',  ( 0.000000000000000000, -1.000000000000000000, 2.220446049250320181E-15 ) ) ;
#16031 = CARTESIAN_POINT ( 'NONE',  ( -0.1749999999999999889, 2.700000000000000178, 0.5999999999999999778 ) ) ;
#16032 = CARTESIAN_POINT ( 'NONE',  ( 2.102728310581320148, -4.241953435693879726, 5.757014351541050345 ) ) ;
#16033 = CARTESIAN_POINT ( 'NONE',  ( 2.013199450439951299, -3.873181699441240244, 5.102405038954985095 ) ) ;
#16034 = CARTESIAN_POINT ( 'NONE',  ( 0.3042893218813449985, 3.050000000000000266, 2.029289321881350361 ) ) ;
#16035 = EDGE_CURVE ( 'NONE', #15023, #3622, #2104, .T. ) ;
#16036 = CARTESIAN_POINT ( 'NONE',  ( 0.1749999999999999889, 9.299999999999998934, 0.4000000000000000222 ) ) ;
#16037 = ORIENTED_EDGE ( 'NONE', *, *, #1455, .F. ) ;
#16038 = CARTESIAN_POINT ( 'NONE',  ( 1.042222075699120287, -0.1245762711864410871, 6.468743694056166227 ) ) ;
#16039 = CARTESIAN_POINT ( 'NONE',  ( -1.145304265383870090, -3.077539021279469988, 6.755972720436099088 ) ) ;
#16040 = VERTEX_POINT ( 'NONE', #9131 ) ;
#16041 = ORIENTED_EDGE ( 'NONE', *, *, #8297, .F. ) ;
#16042 = LINE ( 'NONE', #3341, #12079 ) ;
#16043 = ORIENTED_EDGE ( 'NONE', *, *, #17430, .F. ) ;
#16044 = CARTESIAN_POINT ( 'NONE',  ( -0.4539185741479769276, -3.384127645387189354, 2.390735265170451207 ) ) ;
#16045 = CONTEXT_DEPENDENT_SHAPE_REPRESENTATION ( #9692, #5502 ) ;
#16046 = CARTESIAN_POINT ( 'NONE',  ( 2.171642826483958899, -5.104237288135595740, 6.225392547715717484 ) ) ;
#16047 = CARTESIAN_POINT ( 'NONE',  ( -1.399999999999999911, -5.500000000000000000, 6.100000000000000533 ) ) ;
#16048 = CARTESIAN_POINT ( 'NONE',  ( 1.399999999999999911, 0.5999999999999999778, 6.100000000000000533 ) ) ;
#16049 = EDGE_LOOP ( 'NONE', ( #775, #2655, #7433, #3869 ) ) ;
#16050 = EDGE_CURVE ( 'NONE', #9915, #2194, #8050, .T. ) ;
#16051 = AXIS2_PLACEMENT_3D ( 'NONE', #7925, #3645, #3128 ) ;
#16052 = LINE ( 'NONE', #18033, #17033 ) ;
#16053 = CARTESIAN_POINT ( 'NONE',  ( 1.149999999999999911, 9.299999999999998934, 7.599999999999999645 ) ) ;
#16054 = CARTESIAN_POINT ( 'NONE',  ( 2.016543577558679079, -4.078935417675856101, 4.314702916654005627 ) ) ;
#16055 = EDGE_CURVE ( 'NONE', #12172, #5374, #10718, .T. ) ;
#16056 = CARTESIAN_POINT ( 'NONE',  ( 1.747582379783020778, -0.1156779661016950206, 6.697200745122486865 ) ) ;
#16057 = ORIENTED_EDGE ( 'NONE', *, *, #9354, .F. ) ;
#16058 = ADVANCED_FACE ( 'NONE', ( #16275 ), #16557, .F. ) ;
#16059 = EDGE_LOOP ( 'NONE', ( #11564, #6590 ) ) ;
#16060 = LINE ( 'NONE', #15790, #17736 ) ;
#16061 = CARTESIAN_POINT ( 'NONE',  ( 1.661700935665417544, -5.037501140877957084, 3.038299064334577082 ) ) ;
#16062 = CARTESIAN_POINT ( 'NONE',  ( -0.5385843327681574255, -3.683034516774964295, 2.101338688959530465 ) ) ;
#16063 = ORIENTED_EDGE ( 'NONE', *, *, #7284, .F. ) ;
#16064 = CARTESIAN_POINT ( 'NONE',  ( 0.2023972492402060230, -3.453992510252060111, 2.355265251465770149 ) ) ;
#16065 = DIRECTION ( 'NONE',  ( 1.306144734853129823E-16, -1.000000000000000000, -1.306144734853129823E-16 ) ) ;
#16066 = FACE_OUTER_BOUND ( 'NONE', #2703, .T. ) ;
#16067 = VECTOR ( 'NONE', #9458, 1000.000000000000000 ) ;
#16068 = CARTESIAN_POINT ( 'NONE',  ( 1.642659730162729925, -3.663587104846653730, 3.468508687188663675 ) ) ;
#16070 = EDGE_CURVE ( 'NONE', #7170, #10479, #2301, .T. ) ;
#16069 = CARTESIAN_POINT ( 'NONE',  ( -1.899999999999999911, 11.40000000000000036, 0.5999999999999999778 ) ) ;
#16071 = CARTESIAN_POINT ( 'NONE',  ( 1.124021676335459796, -2.010118636378181112, 2.982013645643220023 ) ) ;
#16072 = AXIS2_PLACEMENT_3D ( 'NONE', #16079, #4682, #14590 ) ;
#16073 = ORIENTED_EDGE ( 'NONE', *, *, #7245, .F. ) ;
#16074 = CARTESIAN_POINT ( 'NONE',  ( -1.399999999999999911, -6.000000000000000000, 5.100000000000000533 ) ) ;
#16075 = LINE ( 'NONE', #13194, #13257 ) ;
#16076 = CARTESIAN_POINT ( 'NONE',  ( 1.233489123281660715, -0.9621456634052125700, 7.049812391606558037 ) ) ;
#16077 = ORIENTED_EDGE ( 'NONE', *, *, #11746, .T. ) ;
#16078 = CARTESIAN_POINT ( 'NONE',  ( -2.281778813005780115, -4.847448931189379806, 5.276394947932169899 ) ) ;
#16079 = CARTESIAN_POINT ( 'NONE',  ( -1.149999999999999911, 6.472933199251450276, 6.846017351831609865 ) ) ;
#16080 = CARTESIAN_POINT ( 'NONE',  ( 1.000000000000000000, -8.000000000000000000, 3.700000000000000178 ) ) ;
#16081 = CARTESIAN_POINT ( 'NONE',  ( -2.306642602145299925, -5.215466101694909540, 5.166805192608490138 ) ) ;
#16082 = ORIENTED_EDGE ( 'NONE', *, *, #3579, .T. ) ;
#16083 = ORIENTED_EDGE ( 'NONE', *, *, #5316, .F. ) ;
#16084 = DIRECTION ( 'NONE',  ( -1.000000000000000000, 0.000000000000000000, -1.850371707708589879E-16 ) ) ;
#16085 = CARTESIAN_POINT ( 'NONE',  ( -0.7999999999998720357, 12.00000000000000000, -2.399999999999999911 ) ) ;
#16086 = EDGE_LOOP ( 'NONE', ( #11724, #12594, #9013, #12424 ) ) ;
#16087 = ADVANCED_FACE ( 'NONE', ( #715 ), #10627, .T. ) ;
#16088 = LINE ( 'NONE', #2098, #5890 ) ;
#16089 = B_SPLINE_CURVE_WITH_KNOTS ( 'NONE', 3,
 ( #3720, #9379, #5081, #9531, #6845, #4988, #15189, #2498, #17930, #6565, #8063, #3595, #10642, #1015, #3683, #14903, #2214, #2315, #9331, #14999, #10926, #16572, #13705, #9616, #826, #12402, #7858, #5171, #10821, #9442, #2416, #6652, #12306, #2582, #18022, #5369, #11009, #15276, #16657, #8232, #13880, #1196, #1475, #165, #5640, #8600, #5545, #2771, #7030, #9988, #14247, #15552, #9893, #11190, #1647, #14327, #11283, #2678, #12488, #15463, #4145, #1285 ),
 .UNSPECIFIED., .F., .F.,
 ( 4, 1, 1, 1, 1, 1, 1, 1, 1, 1, 1, 1, 1, 1, 1, 1, 1, 1, 1, 1, 1, 1, 1, 1, 1, 1, 1, 1, 1, 1, 1, 1, 1, 1, 1, 1, 1, 1, 1, 1, 1, 1, 1, 1, 1, 1, 1, 1, 1, 1, 1, 1, 1, 1, 1, 1, 1, 1, 1, 4 ),
 ( 0.7853981633974479459, 0.8785809963429079827, 0.9717638292883680196, 1.064946662233830166, 1.158129495179289981, 1.251312328124750017, 1.344495161070210054, 1.437677994015669869, 1.530860826961129906, 1.624043659906589943, 1.717226492852049979, 1.810409325797509794, 1.903592158742969609, 1.996774991688429868, 2.089957824633889683, 2.183140657579349941, 2.276323490524809756, 2.369506323470270015, 2.462689156415730274, 2.555871989361190089, 2.649054822306649903, 2.742237655252109718, 2.835420488197569977, 2.928603321143030236, 3.021786154088490051, 3.114968987033949865, 3.208151819979410124, 3.301334652924869939, 3.394517485870330198, 3.487700318815790013, 3.580883151761249827, 3.674065984706710086, 3.767248817652169901, 3.860431650597620390, 3.953614483543079761, 4.046797316488540019, 4.139980149433999834, 4.233162982379460537, 4.326345815324920352, 4.419528648270380167, 4.512711481215839981, 4.605894314161299796, 4.699077147106760499, 4.792259980052219426, 4.885442812997680129, 4.978625645943139943, 5.071808478888599758, 5.164991311834059573, 5.258174144779520276, 5.351356977724980091, 5.444539810670439905, 5.537722643615899720, 5.630905476561360423, 5.724088309506820238, 5.817271142452280053, 5.910453975397739868, 6.003636808343199682, 6.096819641288659497, 6.190002474234119312, 6.283185307179590673 ),
 .UNSPECIFIED. ) ;
#16090 = CARTESIAN_POINT ( 'NONE',  ( -2.121170185508219230, -1.936412895153350133, 3.105085978143999448 ) ) ;
#16091 = CARTESIAN_POINT ( 'NONE',  ( 0.4904671284965613776, -0.6606104644819267291, 2.692290850878278796 ) ) ;
#16092 = CARTESIAN_POINT ( 'NONE',  ( -0.9999999999999978906, 9.099999999999999645, 7.700000000000000178 ) ) ;
#16093 = CARTESIAN_POINT ( 'NONE',  ( -2.276802572547989900, -3.104668185927729862, 4.104251954998810348 ) ) ;
#16095 = EDGE_CURVE ( 'NONE', #9192, #16395, #7952, .T. ) ;
#16094 = CARTESIAN_POINT ( 'NONE',  ( 1.449568901432419343, -5.037500000000000533, 3.250431098567584165 ) ) ;
#16096 = CARTESIAN_POINT ( 'NONE',  ( -1.722199153441400066, -5.095857339597789526, 3.099360556065549943 ) ) ;
#16097 = DIRECTION ( 'NONE',  ( -1.903239470785979823E-16, -1.000000000000000000, 0.000000000000000000 ) ) ;
#16098 = CARTESIAN_POINT ( 'NONE',  ( -1.000000000000000000, 5.799999999999999822, 8.300000000000000711 ) ) ;
#16099 = FACE_OUTER_BOUND ( 'NONE', #13289, .T. ) ;
#16100 = CARTESIAN_POINT ( 'NONE',  ( 2.191755591049679541, -5.346398305084745672, 3.203650300307709475 ) ) ;
#16101 = VERTEX_POINT ( 'NONE', #12294 ) ;
#16102 = CARTESIAN_POINT ( 'NONE',  ( 1.315859850362970151, -5.328211948015590060, 2.737664967889629875 ) ) ;
#16103 = ORIENTED_EDGE ( 'NONE', *, *, #8760, .F. ) ;
#16104 = DIRECTION ( 'NONE',  ( -1.000000000000000000, 0.000000000000000000, 0.000000000000000000 ) ) ;
#16105 = DIRECTION ( 'NONE',  ( 3.018987445473109675E-48, 1.000000000000000000, 2.465190328815659976E-32 ) ) ;
#16106 = ORIENTED_EDGE ( 'NONE', *, *, #9140, .F. ) ;
#16107 = CARTESIAN_POINT ( 'NONE',  ( -0.8429265834919730249, -2.076142624883080323, 2.502678798553459760 ) ) ;
#16108 = LINE ( 'NONE', #3405, #13847 ) ;
#16109 =( NAMED_UNIT ( * ) PLANE_ANGLE_UNIT ( ) SI_UNIT ( $, .RADIAN. ) );
#16110 = CARTESIAN_POINT ( 'NONE',  ( -1.899999999999999911, 2.799999999999999822, 0.6099999999999999867 ) ) ;
#16111 = DIRECTION ( 'NONE',  ( -1.000000000000000000, 2.220446049250309876E-16, 0.000000000000000000 ) ) ;
#16112 = CARTESIAN_POINT ( 'NONE',  ( -0.03714311608457869507, -4.521412895153340550, 7.053160869216429596 ) ) ;
#16113 = CARTESIAN_POINT ( 'NONE',  ( 0.1352600594606461204, -4.199217735477280833, 6.748562071049542865 ) ) ;
#16114 = DIRECTION ( 'NONE',  ( -1.000000000000000000, 0.000000000000000000, 0.000000000000000000 ) ) ;
#16115 = LINE ( 'NONE', #10285, #6490 ) ;
#16116 = ORIENTED_EDGE ( 'NONE', *, *, #14374, .F. ) ;
#16117 = CARTESIAN_POINT ( 'NONE',  ( 0.1749999999999999889, 9.199999999999999289, 0.4000000000000000222 ) ) ;
#16118 = CARTESIAN_POINT ( 'NONE',  ( 1.614765845140360589, -0.1067796610169500227, 5.967758800287426446 ) ) ;
#16119 = CARTESIAN_POINT ( 'NONE',  ( -0.7435598031058080482, -3.030962444702889780, 6.932904947974540377 ) ) ;
#16120 = VERTEX_POINT ( 'NONE', #999 ) ;
#16121 = VERTEX_POINT ( 'NONE', #17914 ) ;
#16122 = LINE ( 'NONE', #11681, #13561 ) ;
#16123 = ORIENTED_EDGE ( 'NONE', *, *, #1578, .T. ) ;
#16124 = DIRECTION ( 'NONE',  ( -0.7071067811865470176, 0.000000000000000000, -0.7071067811865480168 ) ) ;
#16125 = CONTEXT_DEPENDENT_SHAPE_REPRESENTATION ( #3312, #2708 ) ;
#16126 = CARTESIAN_POINT ( 'NONE',  ( -2.130266475405059090, -5.255508474576275901, 3.117337770017961418 ) ) ;
#16127 = LINE ( 'NONE', #4909, #18231 ) ;
#16128 = ADVANCED_FACE ( 'NONE', ( #5259 ), #10913, .T. ) ;
#16129 = CARTESIAN_POINT ( 'NONE',  ( -1.889999999999999902, 3.500000000000000000, -6.185550171619869534E-16 ) ) ;
#16130 = ORIENTED_EDGE ( 'NONE', *, *, #1797, .F. ) ;
#16131 = CARTESIAN_POINT ( 'NONE',  ( 1.065036425888030713, -4.381683165423609694, 6.455163597548602361 ) ) ;
#16132 = CARTESIAN_POINT ( 'NONE',  ( 1.925836318347889931, -0.1112288135593229726, 6.525927015348126581 ) ) ;
#16133 = ORIENTED_EDGE ( 'NONE', *, *, #177, .T. ) ;
#16134 = CARTESIAN_POINT ( 'NONE',  ( 1.057242234132090175, -0.3222457627118650025, 2.597442975781520058 ) ) ;
#16135 = CARTESIAN_POINT ( 'NONE',  ( -0.9707742057416274273, -0.4735169491525429986, 6.508944043303927174 ) ) ;
#16136 = CARTESIAN_POINT ( 'NONE',  ( -2.578017356471871135, -0.5135593220338985354, 5.329826563567776176 ) ) ;
#16137 = ORIENTED_EDGE ( 'NONE', *, *, #9271, .T. ) ;
#16138 = CARTESIAN_POINT ( 'NONE',  ( -2.180207327701300102, -5.506567796610169374, 5.586116916730199833 ) ) ;
#16139 = LINE ( 'NONE', #3440, #17098 ) ;
#16140 = ADVANCED_FACE ( 'NONE', ( #15453 ), #11363, .T. ) ;
#16141 = CARTESIAN_POINT ( 'NONE',  ( -1.899999999999999911, 11.29999999999999893, 1.600000000000000089 ) ) ;
#16142 = PRODUCT_RELATED_PRODUCT_CATEGORY ( 'part', '', ( #6678 ) ) ;
#16143 = EDGE_CURVE ( 'NONE', #404, #2289, #5442, .T. ) ;
#16144 = CARTESIAN_POINT ( 'NONE',  ( 1.945845091385960401, -3.939205687946139900, 2.895339208235789830 ) ) ;
#16145 = VERTEX_POINT ( 'NONE', #11082 ) ;
#16146 = EDGE_CURVE ( 'NONE', #2289, #4403, #11272, .T. ) ;
#16147 = CARTESIAN_POINT ( 'NONE',  ( -2.337178851518210365, -3.011515032774580103, 4.976298214796809560 ) ) ;
#16148 = EDGE_CURVE ( 'NONE', #268, #14546, #8492, .T. ) ;
#16149 = LINE ( 'NONE', #9394, #12323 ) ;
#16150 = DIRECTION ( 'NONE',  ( 2.986159789035700404E-15, -1.110223024625159992E-16, -1.000000000000000000 ) ) ;
#16151 = CARTESIAN_POINT ( 'NONE',  ( 2.045969882616350155, -3.803316834576382366, 4.529973290172005562 ) ) ;
#16152 = CARTESIAN_POINT ( 'NONE',  ( 0.000000000000000000, 0.000000000000000000, 7.700000000000000178 ) ) ;
#16153 = AXIS2_PLACEMENT_3D ( 'NONE', #6239, #683, #11898 ) ;
#16154 = CARTESIAN_POINT ( 'NONE',  ( 0.7778405029480717214, -0.9854339516935015642, 6.599964735094206780 ) ) ;
#16155 = EDGE_LOOP ( 'NONE', ( #13055, #7348 ) ) ;
#16156 = PLANE ( 'NONE',  #2596 ) ;
#16157 = FACE_OUTER_BOUND ( 'NONE', #3476, .T. ) ;
#16158 = CARTESIAN_POINT ( 'NONE',  ( -1.947945325730720434, -1.288181699441250050, 6.502393603230366637 ) ) ;
#16159 = VERTEX_POINT ( 'NONE', #5356 ) ;
#16160 = DIRECTION ( 'NONE',  ( -1.480297366166879989E-15, -2.476791224480685138E-30, -1.000000000000000000 ) ) ;
#16161 = LINE ( 'NONE', #349, #14584 ) ;
#16162 = CIRCLE ( 'NONE', #6114, 0.5999999999999998668 ) ;
#16163 = DIRECTION ( 'NONE',  ( -2.168404344971011235E-15, 1.000000000000000000, 0.000000000000000000 ) ) ;
#16164 = CARTESIAN_POINT ( 'NONE',  ( -1.707817112497179934, -5.188771186440679806, 6.319218296629480314 ) ) ;
#16165 = VERTEX_POINT ( 'NONE', #18178 ) ;
#16166 = EDGE_CURVE ( 'NONE', #10172, #13468, #8405, .T. ) ;
#16167 = VERTEX_POINT ( 'NONE', #8221 ) ;
#16168 = DIRECTION ( 'NONE',  ( -1.224646799147350002E-16, -1.000000000000000000, 0.000000000000000000 ) ) ;
#16169 = LINE ( 'NONE', #1997, #3198 ) ;
#16170 = FACE_OUTER_BOUND ( 'NONE', #3816, .T. ) ;
#16171 = EDGE_CURVE ( 'NONE', #435, #11991, #2947, .T. ) ;
#16172 = EDGE_LOOP ( 'NONE', ( #7758, #16227, #4198, #8381 ) ) ;
#16173 = VECTOR ( 'NONE', #1205, 1000.000000000000000 ) ;
#16174 = VECTOR ( 'NONE', #17204, 1000.000000000000000 ) ;
#16175 = CARTESIAN_POINT ( 'NONE',  ( 0.5803392541454069908, -5.011796459788057767, 2.403119802722881282 ) ) ;
#16176 = CARTESIAN_POINT ( 'NONE',  ( 1.901407128523888934, -2.751502985243430288, 6.551422324754781812 ) ) ;
#16177 = CARTESIAN_POINT ( 'NONE',  ( -1.300000000000000044, 1.592040838891560081E-16, 7.700000000000000178 ) ) ;
#16178 = FACE_OUTER_BOUND ( 'NONE', #8603, .T. ) ;
#16179 = CARTESIAN_POINT ( 'NONE',  ( -0.8748826269293140667, -3.337551068810609589, 2.515205712983220376 ) ) ;
#16180 = VECTOR ( 'NONE', #3988, 1000.000000000000000 ) ;
#16181 = DIRECTION ( 'NONE',  ( 1.000000000000000000, 4.433365283261159518E-17, 1.187916647401989926E-17 ) ) ;
#16183 = VERTEX_POINT ( 'NONE', #2664 ) ;
#16182 = CARTESIAN_POINT ( 'NONE',  ( 1.032615103526660416, -1.284340823081270733, 7.144753513336372208 ) ) ;
#16184 = DIRECTION ( 'NONE',  ( 1.110223024625160090E-15, 1.000000000000000000, 0.000000000000000000 ) ) ;
#16185 = VECTOR ( 'NONE', #1535, 1000.000000000000000 ) ;
#16186 = DIRECTION ( 'NONE',  ( 0.7071067811865474617, 0.7071067811865474617, 0.000000000000000000 ) ) ;
#16187 = AXIS2_PLACEMENT_3D ( 'NONE', #5999, #1653, #16013 ) ;
#16188 = FACE_OUTER_BOUND ( 'NONE', #11608, .T. ) ;
#16189 = FACE_OUTER_BOUND ( 'NONE', #6437, .T. ) ;
#16190 = CARTESIAN_POINT ( 'NONE',  ( 2.651721837666119796, -5.373093220338980736, 4.594045830208265180 ) ) ;
#16191 = ORIENTED_EDGE ( 'NONE', *, *, #18093, .F. ) ;
#16192 = PLANE ( 'NONE',  #11071 ) ;
#16193 = ORIENTED_EDGE ( 'NONE', *, *, #16713, .T. ) ;
#16194 = CARTESIAN_POINT ( 'NONE',  ( 0.7500000000000000000, 6.450000000000000178, 3.200000000000000178 ) ) ;
#16195 = LINE ( 'NONE', #13321, #13862 ) ;
#16196 = AXIS2_PLACEMENT_3D ( 'NONE', #7066, #6954, #11398 ) ;
#16197 = EDGE_CURVE ( 'NONE', #9483, #1501, #12565, .T. ) ;
#16198 = ORIENTED_EDGE ( 'NONE', *, *, #13967, .F. ) ;
#16199 = CARTESIAN_POINT ( 'NONE',  ( -2.316639661709700260, -1.819971453711900056, 4.285359956977770501 ) ) ;
#16200 = AXIS2_PLACEMENT_3D ( 'NONE', #5057, #7654, #10709 ) ;
#16201 = CARTESIAN_POINT ( 'NONE',  ( -1.194742379459959869, -5.475423728813559876, 6.727584234649759409 ) ) ;
#16202 = DIRECTION ( 'NONE',  ( 1.000000000000000000, 2.018587317500279868E-16, 1.110223024625159992E-16 ) ) ;
#16203 = CARTESIAN_POINT ( 'NONE',  ( -2.353343516942199898, -1.773394877135329839, 4.722803042560189901 ) ) ;
#16204 = CARTESIAN_POINT ( 'NONE',  ( 1.026235786675480099, -4.404971453711899798, 6.817920158464540137 ) ) ;
#16205 = MECHANICAL_DESIGN_GEOMETRIC_PRESENTATION_REPRESENTATION (  '', ( #13540 ), #8807 ) ;
#16206 = CARTESIAN_POINT ( 'NONE',  ( 0.8014931112107362976, -1.284340823081270733, 6.590108630558003000 ) ) ;
#16207 = VECTOR ( 'NONE', #15736, 1000.000000000000000 ) ;
#16208 = CARTESIAN_POINT ( 'NONE',  ( 1.000896394980339998, -0.4290254237288140260, 6.829956240957369751 ) ) ;
#16209 = CARTESIAN_POINT ( 'NONE',  ( 0.3042893218813439438, 6.450000000000000178, 2.170710678118660031 ) ) ;
#16210 = CARTESIAN_POINT ( 'NONE',  ( -1.399999999999999911, 0.5999999999999999778, 3.299999999999999822 ) ) ;
#16211 = ORIENTED_EDGE ( 'NONE', *, *, #13850, .F. ) ;
#16212 = CARTESIAN_POINT ( 'NONE',  ( 1.557365740149800226, -0.6207580293448360376, 3.145669832173699998 ) ) ;
#16213 = VECTOR ( 'NONE', #3525, 1000.000000000000000 ) ;
#16214 = CARTESIAN_POINT ( 'NONE',  ( 1.401708661791409849, -4.358394877135329359, 6.590491606684049763 ) ) ;
#16215 = ORIENTED_EDGE ( 'NONE', *, *, #15711, .F. ) ;
#16216 = ORIENTED_EDGE ( 'NONE', *, *, #15501, .F. ) ;
#16217 = LINE ( 'NONE', #17494, #16213 ) ;
#16218 = EDGE_LOOP ( 'NONE', ( #6863, #13159, #16997, #15894 ) ) ;
#16219 = CARTESIAN_POINT ( 'NONE',  ( -1.800000000000000044, 11.40000000000000036, 1.600000000000000089 ) ) ;
#16220 = CIRCLE ( 'NONE', #9420, 0.1500000000000000777 ) ;
#16221 = CARTESIAN_POINT ( 'NONE',  ( -1.192209327851089240, -5.277754237288146300, 2.329031440774910422 ) ) ;
#16222 = CARTESIAN_POINT ( 'NONE',  ( -1.477796163681079911, -0.4824152542372879826, 6.531563725478150673 ) ) ;
#16223 = ORIENTED_EDGE ( 'NONE', *, *, #874, .T. ) ;
#16224 = AXIS2_PLACEMENT_3D ( 'NONE', #4543, #3266, #14292 ) ;
#16225 = CARTESIAN_POINT ( 'NONE',  ( -1.865240315818168959, -3.450151633892079239, 3.842223568244830467 ) ) ;
#16226 = CARTESIAN_POINT ( 'NONE',  ( -0.7998959936908373036, -0.4646186440677965712, 7.230419212249866945 ) ) ;
#16227 = ORIENTED_EDGE ( 'NONE', *, *, #1354, .F. ) ;
#16228 = CARTESIAN_POINT ( 'NONE',  ( 1.428515267734870031, -0.3311440677966109858, 2.829745655876919841 ) ) ;
#16229 = CARTESIAN_POINT ( 'NONE',  ( 1.596341326794969984, -0.3355932203389830337, 2.970780074643809776 ) ) ;
#16230 = AXIS2_PLACEMENT_3D ( 'NONE', #4973, #5357, #5260 ) ;
#16231 = EDGE_LOOP ( 'NONE', ( #12854, #6791 ) ) ;
#16232 = CARTESIAN_POINT ( 'NONE',  ( -0.3171869470818471370, -0.4557203389830515317, 7.334814496515233095 ) ) ;
#16233 = ORIENTED_EDGE ( 'NONE', *, *, #6636, .F. ) ;
#16234 = CARTESIAN_POINT ( 'NONE',  ( 0.9150601050661639757, -5.430932203389830626, 6.868218666554230190 ) ) ;
#16235 = CARTESIAN_POINT ( 'NONE',  ( -1.250000000000000000, 7.799999999999999822, 7.599999999999999645 ) ) ;
#16236 = DIRECTION ( 'NONE',  ( 3.172065784643300034E-16, -1.000000000000000000, -1.586032892321649771E-16 ) ) ;
#16237 = CARTESIAN_POINT ( 'NONE',  ( 0.7093417302541469294, -5.435381355932199732, 6.943956659919690466 ) ) ;
#16238 = CARTESIAN_POINT ( 'NONE',  ( -2.574214976178951009, -3.403575057315514130, 4.054607910322786779 ) ) ;
#16239 = VERTEX_POINT ( 'NONE', #16914 ) ;
#16240 = CARTESIAN_POINT ( 'NONE',  ( -0.4446501070882830087, -4.952022267818760426, 2.379695998155090031 ) ) ;
#16241 = CIRCLE ( 'NONE', #8278, 0.2500000000000002220 ) ;
#16242 = CARTESIAN_POINT ( 'NONE',  ( 0.3159454637157339540, -2.615614131873679860, 7.032150113402090064 ) ) ;
#16243 = SPHERICAL_SURFACE ( 'NONE', #15291, 1.016666666666670160 ) ;
#16244 = CYLINDRICAL_SURFACE ( 'NONE', #1961, 0.4166666666666670737 ) ;
#16245 = CARTESIAN_POINT ( 'NONE',  ( 1.203420131881999477, -4.059488005747546424, 6.363334551077796775 ) ) ;
#16246 = FACE_OUTER_BOUND ( 'NONE', #4466, .T. ) ;
#16247 = DIRECTION ( 'NONE',  ( 0.000000000000000000, 0.000000000000000000, 1.000000000000000000 ) ) ;
#16248 = CARTESIAN_POINT ( 'NONE',  ( 1.937109463115360253, -2.173136654396201184, 4.019920026366761157 ) ) ;
#16249 = VERTEX_POINT ( 'NONE', #4134 ) ;
#16250 = DIRECTION ( 'NONE',  ( 1.000000000000000000, 0.000000000000000000, 0.000000000000000000 ) ) ;
#16251 = EDGE_CURVE ( 'NONE', #1501, #5435, #8587, .T. ) ;
#16252 = CARTESIAN_POINT ( 'NONE',  ( -0.009452110982655099330, -0.5998079552954631577, 2.649999999999998579 ) ) ;
#16253 = CARTESIAN_POINT ( 'NONE',  ( 2.501774541437309374, -0.7758393570989061683, 5.585572039315881199 ) ) ;
#16254 = EDGE_CURVE ( 'NONE', #17710, #3506, #9975, .T. ) ;
#16255 = VERTEX_POINT ( 'NONE', #15542 ) ;
#16256 = VECTOR ( 'NONE', #14803, 1000.000000000000000 ) ;
#16257 = LINE ( 'NONE', #2084, #14097 ) ;
#16258 = DIRECTION ( 'NONE',  ( -3.700743415417199972E-16, 1.000000000000000000, 3.581736239852565328E-31 ) ) ;
#16259 = DIRECTION ( 'NONE',  ( -0.7049180327868849183, 0.7092887755011130224, 8.531426931033447850E-16 ) ) ;
#16260 = CARTESIAN_POINT ( 'NONE',  ( -1.889104232906369862, -5.255508474576269684, 3.296507079072529933 ) ) ;
#16261 = ORIENTED_EDGE ( 'NONE', *, *, #7213, .T. ) ;
#16262 = EDGE_LOOP ( 'NONE', ( #1716, #13854, #14699, #14991 ) ) ;
#16263 = DIRECTION ( 'NONE',  ( 0.000000000000000000, 0.000000000000000000, -1.000000000000000000 ) ) ;
#16264 = DIRECTION ( 'NONE',  ( -1.000000000000000000, 0.000000000000000000, 0.000000000000000000 ) ) ;
#16265 = CARTESIAN_POINT ( 'NONE',  ( -0.5500000000000000444, 2.050000000000000266, 3.600000000000000089 ) ) ;
#16266 = VERTEX_POINT ( 'NONE', #2844 ) ;
#16267 = CARTESIAN_POINT ( 'NONE',  ( -1.526871680339578541, -5.559957627118640389, 3.327650196883449762 ) ) ;
#16268 = CARTESIAN_POINT ( 'NONE',  ( -1.524497189778160289, -2.801920438179980710, 6.872331008700187205 ) ) ;
#16269 = CARTESIAN_POINT ( 'NONE',  ( 1.319613955262859850, -5.028306595106927901, 2.740497729816110173 ) ) ;
#16270 = CARTESIAN_POINT ( 'NONE',  ( 2.647661051184980519, -2.541908390648840665, 4.518328177639069132 ) ) ;
#16271 = LINE ( 'NONE', #17629, #3478 ) ;
#16272 = DIRECTION ( 'NONE',  ( -1.000000000000000000, 0.000000000000000000, 6.123233995736769734E-17 ) ) ;
#16273 = VECTOR ( 'NONE', #1560, 1000.000000000000000 ) ;
#16274 = CARTESIAN_POINT ( 'NONE',  ( 0.3752419433107369584, -4.175929447188989840, 7.023346545710360544 ) ) ;
#16275 = FACE_OUTER_BOUND ( 'NONE', #4703, .T. ) ;
#16276 = LINE ( 'NONE', #915, #15664 ) ;
#16278 = ORIENTED_EDGE ( 'NONE', *, *, #16891, .F. ) ;
#16277 = CARTESIAN_POINT ( 'NONE',  ( 1.315254646989809872, -2.821367850108300157, 7.005042061779697349 ) ) ;
#16279 = ADVANCED_FACE ( 'NONE', ( #7015 ), #14141, .T. ) ;
#16280 = CARTESIAN_POINT ( 'NONE',  ( 1.899999999999999911, 7.299999999999999822, 1.600000000000000089 ) ) ;
#16281 = CARTESIAN_POINT ( 'NONE',  ( 0.4360591020457930123, -0.3088983050847460277, 2.387347919655840034 ) ) ;
#16282 = EDGE_CURVE ( 'NONE', #17446, #1300, #71, .T. ) ;
#16283 = CARTESIAN_POINT ( 'NONE',  ( 0.2818998297622880012, -1.354205687946139935, 7.036509827384409554 ) ) ;
#16284 = CARTESIAN_POINT ( 'NONE',  ( -1.661700935788390066, -0.5625000000000000000, 3.038299064211610112 ) ) ;
#16285 = CARTESIAN_POINT ( 'NONE',  ( 0.03000000000000110217, 11.40000000000000036, 1.600000000000000089 ) ) ;
#16286 = ORIENTED_EDGE ( 'NONE', *, *, #8822, .T. ) ;
#16287 = CARTESIAN_POINT ( 'NONE',  ( -0.9000000000000000222, -10.00000000000000000, 3.799999999999999822 ) ) ;
#16288 = ORIENTED_EDGE ( 'NONE', *, *, #6417, .T. ) ;
#16289 = DIRECTION ( 'NONE',  ( 1.000000000000000000, 0.000000000000000000, -2.379049338482479710E-16 ) ) ;
#16290 = VECTOR ( 'NONE', #2164, 1000.000000000000000 ) ;
#16291 = FACE_OUTER_BOUND ( 'NONE', #10900, .T. ) ;
#16292 = EDGE_LOOP ( 'NONE', ( #638, #3554, #11525, #5472 ) ) ;
#16293 = ORIENTED_EDGE ( 'NONE', *, *, #16987, .T. ) ;
#16294 = CARTESIAN_POINT ( 'NONE',  ( 0.7678268402137939930, -2.867944426684879922, 6.924676972266129660 ) ) ;
#16295 = EDGE_CURVE ( 'NONE', #6842, #13656, #16725, .T. ) ;
#16296 = DIRECTION ( 'NONE',  ( 7.401486830834380223E-16, -4.695600626315540288E-31, 1.000000000000000000 ) ) ;
#16297 = CARTESIAN_POINT ( 'NONE',  ( -0.8570167067220350043, -5.582203389830509899, 2.508190348879359988 ) ) ;
#16298 = PLANE ( 'NONE',  #14377 ) ;
#16299 = CARTESIAN_POINT ( 'NONE',  ( 0.3413183941262679655, -2.914521003261450360, 7.028571974690709823 ) ) ;
#16300 = CARTESIAN_POINT ( 'NONE',  ( 2.260890494820590124, -4.055647129387580208, 4.046455925041149371 ) ) ;
#16301 = CARTESIAN_POINT ( 'NONE',  ( 2.052456847059610734, -2.565196678937129438, 4.748194746458525017 ) ) ;
#16302 = EDGE_CURVE ( 'NONE', #6821, #14368, #1384, .T. ) ;
#16303 = CARTESIAN_POINT ( 'NONE',  ( -0.5999999999999999778, 11.40000000000000036, 7.700000000000000178 ) ) ;
#16304 = EDGE_LOOP ( 'NONE', ( #3234, #18058, #3374, #12771 ) ) ;
#16305 = LINE ( 'NONE', #329, #7929 ) ;
#16306 = LINE ( 'NONE', #17767, #430 ) ;
#16307 = CARTESIAN_POINT ( 'NONE',  ( 2.100188519621589922, -4.009070552810999999, 3.637948273607370275 ) ) ;
#16308 = ORIENTED_EDGE ( 'NONE', *, *, #16840, .F. ) ;
#16309 = ORIENTED_EDGE ( 'NONE', *, *, #6740, .T. ) ;
#16310 = EDGE_CURVE ( 'NONE', #16755, #9388, #10998, .T. ) ;
#16311 = LINE ( 'NONE', #13160, #7358 ) ;
#16312 = VERTEX_POINT ( 'NONE', #9695 ) ;
#16313 = LINE ( 'NONE', #11876, #9499 ) ;
#16314 = SHAPE_DEFINITION_REPRESENTATION ( #1222, #2146 ) ;
#16315 = CARTESIAN_POINT ( 'NONE',  ( -0.2469343877495291661, -5.295550847457634269, 2.057675570509529539 ) ) ;
#16316 = ADVANCED_FACE ( 'NONE', ( #3952 ), #13867, .T. ) ;
#16317 = CARTESIAN_POINT ( 'NONE',  ( -1.899999999999999911, 11.25000000000000000, 7.649999999999999467 ) ) ;
#16318 = ORIENTED_EDGE ( 'NONE', *, *, #18174, .T. ) ;
#16319 = LINE ( 'NONE', #2442, #18229 ) ;
#16320 = CARTESIAN_POINT ( 'NONE',  ( 1.632144308286169965, -4.288530012270460823, 5.945394234592866312 ) ) ;
#16321 = CARTESIAN_POINT ( 'NONE',  ( 1.128670402850170174, -0.4290254237288141370, 7.101865548313628373 ) ) ;
#16322 = ADVANCED_FACE ( 'NONE', ( #8854 ), #17171, .T. ) ;
#16323 = ORIENTED_EDGE ( 'NONE', *, *, #9132, .T. ) ;
#16324 = CARTESIAN_POINT ( 'NONE',  ( -2.578017356471871135, -0.2135593220338991571, 5.329826563567776176 ) ) ;
#16325 = ORIENTED_EDGE ( 'NONE', *, *, #11474, .T. ) ;
#16326 = CARTESIAN_POINT ( 'NONE',  ( -0.3743405594629430344, -5.457627118644070130, 7.023440622744399953 ) ) ;
#16327 = CARTESIAN_POINT ( 'NONE',  ( 1.670747152266691016, -0.4963810343603142217, 3.047345280935851441 ) ) ;
#16328 = CARTESIAN_POINT ( 'NONE',  ( -0.009452110982655708218, -0.5998079552954630467, 2.350000000000000089 ) ) ;
#16329 = CARTESIAN_POINT ( 'NONE',  ( 1.882879255550339082, -0.4963798976394455664, 2.835213315261639000 ) ) ;
#16330 = EDGE_LOOP ( 'NONE', ( #1626, #13416, #13784, #11804 ) ) ;
#16331 = LINE ( 'NONE', #8013, #8746 ) ;
#16332 = VECTOR ( 'NONE', #12739, 1000.000000000000000 ) ;
#16333 = CARTESIAN_POINT ( 'NONE',  ( -1.928817277882840076, -4.455388906648449776, 6.048484184565969812 ) ) ;
#16334 = LINE ( 'NONE', #7816, #2255 ) ;
#16335 = CARTESIAN_POINT ( 'NONE',  ( -1.800000000000000044, 0.5999999999999999778, 7.550000000000000711 ) ) ;
#16336 = CARTESIAN_POINT ( 'NONE',  ( 1.043047520545210105, -4.082776294035843634, 6.468319459971126228 ) ) ;
#16337 = DIRECTION ( 'NONE',  ( -1.480297366166879989E-16, 0.000000000000000000, 1.000000000000000000 ) ) ;
#16338 = FACE_OUTER_BOUND ( 'NONE', #2078, .T. ) ;
#16339 = CARTESIAN_POINT ( 'NONE',  ( 0.2302241296434710538, -1.893677194936738806, 2.659926792304259990 ) ) ;
#16340 = EDGE_LOOP ( 'NONE', ( #5101, #8480, #15543, #16610 ) ) ;
#16341 = DIRECTION ( 'NONE',  ( 4.440892098500620245E-16, 1.000000000000000000, 2.220446049250309876E-16 ) ) ;
#16342 = CARTESIAN_POINT ( 'NONE',  ( -1.250000000000000000, 0.5999999999999999778, 6.100000000000000533 ) ) ;
#16343 = CARTESIAN_POINT ( 'NONE',  ( 0.1953673232040119001, -0.6247245358507567126, 2.648920247487680513 ) ) ;
#16344 = CARTESIAN_POINT ( 'NONE',  ( -0.6265155281652096120, -2.708767285026830951, 7.278874170247493502 ) ) ;
#16345 = ORIENTED_EDGE ( 'NONE', *, *, #4313, .F. ) ;
#16346 = DIRECTION ( 'NONE',  ( 1.000000000000000000, 0.000000000000000000, -4.265713465516738421E-15 ) ) ;
#16347 = CARTESIAN_POINT ( 'NONE',  ( -1.197297565406129971, -1.517223705964160008, 6.726135293448209929 ) ) ;
#16348 = CARTESIAN_POINT ( 'NONE',  ( -1.670747221194380128, -5.103620102360550526, 3.047345349617600174 ) ) ;
#16349 = EDGE_CURVE ( 'NONE', #1943, #18075, #4936, .T. ) ;
#16350 = CARTESIAN_POINT ( 'NONE',  ( 0.2812789908084389889, -5.144279661016950556, 7.036533610117280624 ) ) ;
#16351 = ORIENTED_EDGE ( 'NONE', *, *, #10780, .F. ) ;
#16352 = VERTEX_POINT ( 'NONE', #10329 ) ;
#16353 = CARTESIAN_POINT ( 'NONE',  ( -1.250000000000000000, 3.500000000000000000, 5.100000000000000533 ) ) ;
#16354 = DIRECTION ( 'NONE',  ( 1.224646799147350002E-16, -1.000000000000000000, -6.123233995736779594E-17 ) ) ;
#16355 = CARTESIAN_POINT ( 'NONE',  ( 1.850000000000000089, -6.000000000000000000, 2.299999999999999822 ) ) ;
#16356 = ORIENTED_EDGE ( 'NONE', *, *, #155, .T. ) ;
#16357 = CARTESIAN_POINT ( 'NONE',  ( -2.180207327701300102, -5.506567796610169374, 5.586116916730199833 ) ) ;
#16358 = CARTESIAN_POINT ( 'NONE',  ( 1.392767620582681332, -3.570433951693503527, 2.440948861123688474 ) ) ;
#16359 = CARTESIAN_POINT ( 'NONE',  ( 1.327748599278329777, -0.4480353997208160188, 2.745754414290000334 ) ) ;
#16360 = CARTESIAN_POINT ( 'NONE',  ( -0.7785957873162068221, -3.659746228486683073, 2.162894899107379754 ) ) ;
#16361 = DIRECTION ( 'NONE',  ( 0.000000000000000000, 0.000000000000000000, 1.000000000000000000 ) ) ;
#16362 = MECHANICAL_DESIGN_GEOMETRIC_PRESENTATION_REPRESENTATION (  '', ( #6009 ), #3028 ) ;
#16363 = DIRECTION ( 'NONE',  ( -8.971499188890150495E-16, 0.000000000000000000, -1.000000000000000000 ) ) ;
#16364 = EDGE_CURVE ( 'NONE', #17345, #7849, #8666, .T. ) ;
#16365 = CARTESIAN_POINT ( 'NONE',  ( -1.265407828724339989, -3.290974492234040483, 2.715689360385570073 ) ) ;
#16366 = DIRECTION ( 'NONE',  ( 3.700743415417190112E-16, 1.000000000000000000, 0.000000000000000000 ) ) ;
#16367 = CARTESIAN_POINT ( 'NONE',  ( -0.9499999999999999556, 2.299999999999999822, 7.599999999999999645 ) ) ;
#16369 = ORIENTED_EDGE ( 'NONE', *, *, #13107, .T. ) ;
#16368 = CARTESIAN_POINT ( 'NONE',  ( 2.065789008933020199, -2.728214696955149510, 6.366022047745297563 ) ) ;
#16370 = CARTESIAN_POINT ( 'NONE',  ( 1.699999999999999956, 2.299999999999999822, 7.700000000000000178 ) ) ;
#16371 = CARTESIAN_POINT ( 'NONE',  ( 0.07299321914061039640, -0.3014830508474579673, 2.350000000000000089 ) ) ;
#16372 = CARTESIAN_POINT ( 'NONE',  ( -1.854177340199669954, -1.610376859117309989, 6.149404042554720284 ) ) ;
#16373 = CARTESIAN_POINT ( 'NONE',  ( -2.286166334984490067, -0.5135593220338989795, 5.258525443163870605 ) ) ;
#16374 = CARTESIAN_POINT ( 'NONE',  ( -0.4478021372196528960, -0.2909039927201509945, 2.380136890750930156 ) ) ;
#16375 = CARTESIAN_POINT ( 'NONE',  ( 2.416676968769261080, -5.395338983050850246, 5.796598111919825769 ) ) ;
#16376 = ORIENTED_EDGE ( 'NONE', *, *, #9976, .T. ) ;
#16377 = DIRECTION ( 'NONE',  ( 0.000000000000000000, 0.000000000000000000, 1.000000000000000000 ) ) ;
#16378 = ORIENTED_EDGE ( 'NONE', *, *, #10067, .T. ) ;
#16379 = CARTESIAN_POINT ( 'NONE',  ( 1.889999999999999902, 7.299999999999999822, -1.002722375122780079E-16 ) ) ;
#16380 = CARTESIAN_POINT ( 'NONE',  ( 1.850000000000000089, 11.25000000000000000, 8.300000000000000711 ) ) ;
#16381 = ADVANCED_FACE ( 'NONE', ( #7543 ), #425, .T. ) ;
#16382 = VERTEX_POINT ( 'NONE', #13188 ) ;
#16383 = CARTESIAN_POINT ( 'NONE',  ( -1.741913176380149864, -1.959701183441629802, 3.117443785062560035 ) ) ;
#16384 = ADVANCED_FACE ( 'NONE', ( #17249 ), #154, .T. ) ;
#16385 = LINE ( 'NONE', #16474, #7626 ) ;
#16386 = DIRECTION ( 'NONE',  ( 4.336808689942013792E-16, -1.000000000000000000, 0.000000000000000000 ) ) ;
#16387 = EDGE_CURVE ( 'NONE', #13202, #8663, #17343, .T. ) ;
#16388 = DIRECTION ( 'NONE',  ( 1.224646799147350002E-16, -1.000000000000000000, -6.123233995736769734E-17 ) ) ;
#16389 = ADVANCED_FACE ( 'NONE', ( #3024 ), #11815, .T. ) ;
#16390 = CARTESIAN_POINT ( 'NONE',  ( 2.301223891756920104, -2.611773255513699876, 5.193066210047949660 ) ) ;
#16391 = DIRECTION ( 'NONE',  ( 6.123233995736769734E-17, 9.462128050782581713E-15, 1.000000000000000000 ) ) ;
#16392 = CARTESIAN_POINT ( 'NONE',  ( -0.8735826871841183561, -1.493935417675870791, 6.557889967484691773 ) ) ;
#16393 = CARTESIAN_POINT ( 'NONE',  ( -1.399999999999999911, -5.000000000000000000, 3.299999999999999822 ) ) ;
#16394 = CARTESIAN_POINT ( 'NONE',  ( -1.687197751398160861, -0.5672554343907065810, 2.639290338773708999 ) ) ;
#16395 = VERTEX_POINT ( 'NONE', #15990 ) ;
#16396 = CARTESIAN_POINT ( 'NONE',  ( 1.635135312535000107, -0.5029574999466160934, 3.082160985277540011 ) ) ;
#16397 = CARTESIAN_POINT ( 'NONE',  ( -1.000000000000000000, -5.500000000000000000, 6.100000000000000533 ) ) ;
#16398 = LINE ( 'NONE', #9350, #3658 ) ;
#16399 = VECTOR ( 'NONE', #16377, 1000.000000000000000 ) ;
#16400 = ORIENTED_EDGE ( 'NONE', *, *, #8590, .F. ) ;
#16401 = VERTEX_POINT ( 'NONE', #5800 ) ;
#16402 = VERTEX_POINT ( 'NONE', #10143 ) ;
#16403 = CARTESIAN_POINT ( 'NONE',  ( -2.287919158821179799, -4.548542059801598647, 5.251517552016938595 ) ) ;
#16404 = CARTESIAN_POINT ( 'NONE',  ( 1.943632316591230147, -5.046398305084740521, 3.373048379518159834 ) ) ;
#16405 = EDGE_CURVE ( 'NONE', #12255, #5954, #13020, .T. ) ;
#16406 = VERTEX_POINT ( 'NONE', #16069 ) ;
#16407 = CARTESIAN_POINT ( 'NONE',  ( -2.035218756299248977, -4.781424942684484591, 2.996768277952679860 ) ) ;
#16408 = LINE ( 'NONE', #6592, #17346 ) ;
#16409 = CARTESIAN_POINT ( 'NONE',  ( -2.308170020371289599, -1.726818300558750074, 5.159452766389659217 ) ) ;
#16410 = CARTESIAN_POINT ( 'NONE',  ( 1.750316316486830059, -0.04004237288135630013, 3.126818518378580158 ) ) ;
#16411 = ORIENTED_EDGE ( 'NONE', *, *, #4482, .F. ) ;
#16412 = ORIENTED_EDGE ( 'NONE', *, *, #4278, .F. ) ;
#16413 = CARTESIAN_POINT ( 'NONE',  ( -0.7998959936908373036, -0.1646186440677970542, 7.230419212249866945 ) ) ;
#16414 = VERTEX_POINT ( 'NONE', #17083 ) ;
#16415 = PLANE ( 'NONE',  #9413 ) ;
#16416 = CARTESIAN_POINT ( 'NONE',  ( -2.500000000000000000, 7.299999999999999822, 0.6099999999999999867 ) ) ;
#16417 = CARTESIAN_POINT ( 'NONE',  ( 2.239137794397009440, -0.6128213390808880945, 3.975425900939169921 ) ) ;
#16418 = CARTESIAN_POINT ( 'NONE',  ( -0.1565249325564300187, -5.453177966101690366, 7.048192310558509810 ) ) ;
#16419 = VECTOR ( 'NONE', #14950, 1000.000000000000000 ) ;
#16420 = CARTESIAN_POINT ( 'NONE',  ( -2.159308672244651284, -4.754295778036219389, 6.242886823772542115 ) ) ;
#16421 = EDGE_CURVE ( 'NONE', #14832, #18253, #4490, .T. ) ;
#16422 = ORIENTED_EDGE ( 'NONE', *, *, #4561, .T. ) ;
#16423 = CARTESIAN_POINT ( 'NONE',  ( -2.500000000000000000, 9.199999999999999289, 0.6099999999999999867 ) ) ;
#16424 = CARTESIAN_POINT ( 'NONE',  ( -2.350542563031990273, -4.595118636378179744, 4.817027120179790067 ) ) ;
#16425 = CARTESIAN_POINT ( 'NONE',  ( -2.632587027711260852, -4.940602084342534894, 4.364441905910590336 ) ) ;
#16426 = LINE ( 'NONE', #3731, #12607 ) ;
#16427 = DIRECTION ( 'NONE',  ( -2.220446049250309876E-16, -1.000000000000000000, 1.268826313857319964E-16 ) ) ;
#16428 = CARTESIAN_POINT ( 'NONE',  ( -1.436030008293460503, -4.408812330071866015, 6.167214932417466322 ) ) ;
#16429 = CARTESIAN_POINT ( 'NONE',  ( 0.1749999999999999889, 7.900000000000000355, 0.5999999999999999778 ) ) ;
#16430 = LINE ( 'NONE', #10882, #3217 ) ;
#16431 = CARTESIAN_POINT ( 'NONE',  ( 2.002297259025890064, -2.312866384125929820, 5.153549919110900213 ) ) ;
#16432 = ORIENTED_EDGE ( 'NONE', *, *, #207, .F. ) ;
#16433 = DIRECTION ( 'NONE',  ( 0.000000000000000000, 1.000000000000000000, 0.000000000000000000 ) ) ;
#16434 = FACE_OUTER_BOUND ( 'NONE', #16330, .T. ) ;
#16435 = AXIS2_PLACEMENT_3D ( 'NONE', #14524, #17378, #10788 ) ;
#16436 = DIRECTION ( 'NONE',  ( -1.000000000000000000, 0.000000000000000000, 0.000000000000000000 ) ) ;
#16437 = CARTESIAN_POINT ( 'NONE',  ( 2.623186471072028514, -2.219713230972778728, 4.297499775172036962 ) ) ;
#16438 = EDGE_LOOP ( 'NONE', ( #13678, #7740, #11209, #6033 ) ) ;
#16439 = DIRECTION ( 'NONE',  ( 0.000000000000000000, 0.000000000000000000, -1.000000000000000000 ) ) ;
#16440 = LINE ( 'NONE', #14970, #13628 ) ;
#16441 = CARTESIAN_POINT ( 'NONE',  ( 1.432215783582721613, -5.113135593220339281, 6.170863372171116801 ) ) ;
#16442 = ORIENTED_EDGE ( 'NONE', *, *, #17371, .F. ) ;
#16443 = ORIENTED_EDGE ( 'NONE', *, *, #15544, .T. ) ;
#16444 = FACE_OUTER_BOUND ( 'NONE', #13192, .T. ) ;
#16445 = CARTESIAN_POINT ( 'NONE',  ( 0.3367924244280819934, 2.254758922476410188, 7.700000000000000178 ) ) ;
#16446 = ORIENTED_EDGE ( 'NONE', *, *, #4561, .F. ) ;
#16447 = CARTESIAN_POINT ( 'NONE',  ( 2.286166334984490067, -5.386440677966100488, 5.258525443163859947 ) ) ;
#16448 = CARTESIAN_POINT ( 'NONE',  ( 2.644456467089558949, -3.803316834576382366, 4.476474416072626639 ) ) ;
#16449 = DIRECTION ( 'NONE',  ( 1.224646799147350002E-16, -1.000000000000000000, -6.123233995736779594E-17 ) ) ;
#16450 = CIRCLE ( 'NONE', #4604, 0.2000000000000000111 ) ;
#16451 = DIRECTION ( 'NONE',  ( 3.652293603810800245E-15, 1.332267629550190018E-15, -1.000000000000000000 ) ) ;
#16452 = DIRECTION ( 'NONE',  ( 1.000000000000000000, 4.014365738757630620E-15, 5.017957173447030386E-16 ) ) ;
#16453 = CARTESIAN_POINT ( 'NONE',  ( -1.074829861819750043, -3.314262780522330143, 2.606322265575609975 ) ) ;
#16454 = ADVANCED_FACE ( 'NONE', ( #3293 ), #15025, .T. ) ;
#16455 = DIRECTION ( 'NONE',  ( 1.000000000000000000, 0.000000000000000000, 0.000000000000000000 ) ) ;
#16456 = CARTESIAN_POINT ( 'NONE',  ( 0.1749999999999999889, 7.900000000000000355, 0.4000000000000000222 ) ) ;
#16458 = ORIENTED_EDGE ( 'NONE', *, *, #11178, .T. ) ;
#16457 = CARTESIAN_POINT ( 'NONE',  ( 0.2683982510036849733, -2.192584066324520187, 2.059720455735791322 ) ) ;
#16459 = DIRECTION ( 'NONE',  ( 1.224646799147350002E-16, -1.000000000000000000, -6.123233995736769734E-17 ) ) ;
#16460 = CARTESIAN_POINT ( 'NONE',  ( -1.750000000000000000, 0.5999999999999999778, 7.599999999999999645 ) ) ;
#16461 = CARTESIAN_POINT ( 'NONE',  ( 2.126557263589630153, -2.448755237495689574, 3.691783806836010040 ) ) ;
#16462 = VECTOR ( 'NONE', #7421, 1000.000000000000000 ) ;
#16463 = CARTESIAN_POINT ( 'NONE',  ( 0.009303514085960742572, -5.002547179689483592, 2.316528937223460982 ) ) ;
#16464 = DIRECTION ( 'NONE',  ( -1.000000000000000000, 0.000000000000000000, 7.401486830834390084E-16 ) ) ;
#16465 = CARTESIAN_POINT ( 'NONE',  ( -1.596341326794979976, -5.564406779661021041, 2.970780074643819990 ) ) ;
#16466 = ORIENTED_EDGE ( 'NONE', *, *, #15164, .F. ) ;
#16467 = AXIS2_PLACEMENT_3D ( 'NONE', #5555, #16931, #18199 ) ;
#16468 = CARTESIAN_POINT ( 'NONE',  ( -1.899999999999999911, 0.5999999999999999778, 7.599999999999999645 ) ) ;
#16469 = CARTESIAN_POINT ( 'NONE',  ( -0.5999999999999999778, 10.80000000000000071, 7.599999999999999645 ) ) ;
#16470 = ORIENTED_EDGE ( 'NONE', *, *, #13350, .T. ) ;
#16471 = VECTOR ( 'NONE', #1726, 1000.000000000000000 ) ;
#16472 = CARTESIAN_POINT ( 'NONE',  ( -1.286937324407759986, -3.589881363621809651, 2.729584305145209999 ) ) ;
#16473 = SHAPE_REPRESENTATION ( 'Latch Lock Pin Wire', ( #17681 ), #12699 ) ;
#16474 = CARTESIAN_POINT ( 'NONE',  ( 2.500000000000000000, 7.299999999999999822, 1.600000000000000089 ) ) ;
#16475 = LINE ( 'NONE', #9538, #3167 ) ;
#16476 = DIRECTION ( 'NONE',  ( -2.018587317500279868E-16, 1.000000000000000000, 0.000000000000000000 ) ) ;
#16477 = DIRECTION ( 'NONE',  ( 0.000000000000000000, -1.000000000000000000, 0.000000000000000000 ) ) ;
#16478 = VECTOR ( 'NONE', #11059, 1000.000000000000000 ) ;
#16479 = CARTESIAN_POINT ( 'NONE',  ( -1.236334101859210000, -2.029566048306499670, 2.697445712080720259 ) ) ;
#16480 = AXIS2_PLACEMENT_3D ( 'NONE', #3014, #10209, #15976 ) ;
#16481 = DIRECTION ( 'NONE',  ( -3.700743415417195042E-15, -3.289549702593060375E-15, 1.000000000000000000 ) ) ;
#16482 = CARTESIAN_POINT ( 'NONE',  ( -1.616473591439278712, -1.610376859117309767, 5.965667796385567101 ) ) ;
#16483 = CARTESIAN_POINT ( 'NONE',  ( 2.500000000000000000, 1.148961478048669885E-16, -2.399999999999999911 ) ) ;
#16484 = CIRCLE ( 'NONE', #8508, 1.016666666666670160 ) ;
#16485 = CIRCLE ( 'NONE', #10872, 0.6099999999999999867 ) ;
#16486 = CARTESIAN_POINT ( 'NONE',  ( -0.4478021372196530070, -0.2909039927201509945, 2.380136890750930156 ) ) ;
#16487 = ORIENTED_EDGE ( 'NONE', *, *, #1464, .T. ) ;
#16488 = EDGE_CURVE ( 'NONE', #11655, #14407, #3368, .T. ) ;
#16489 = DIRECTION ( 'NONE',  ( 0.000000000000000000, 1.000000000000000000, 0.000000000000000000 ) ) ;
#16490 = VECTOR ( 'NONE', #4365, 1000.000000000000000 ) ;
#16491 = CARTESIAN_POINT ( 'NONE',  ( -1.850000000000000089, 11.25000000000000000, 7.700000000000000178 ) ) ;
#16492 = DIRECTION ( 'NONE',  ( 0.000000000000000000, 0.000000000000000000, -1.000000000000000000 ) ) ;
#16493 = VERTEX_POINT ( 'NONE', #17440 ) ;
#16494 = ADVANCED_FACE ( 'NONE', ( #15799 ), #4758, .T. ) ;
#16495 = ORIENTED_EDGE ( 'NONE', *, *, #8445, .F. ) ;
#16496 = EDGE_CURVE ( 'NONE', #8454, #12005, #5894, .T. ) ;
#16497 = VECTOR ( 'NONE', #14679, 1000.000000000000000 ) ;
#16498 = ORIENTED_EDGE ( 'NONE', *, *, #10185, .T. ) ;
#16499 = DIRECTION ( 'NONE',  ( 1.110223024625159992E-16, 0.000000000000000000, -1.000000000000000000 ) ) ;
#16500 = CARTESIAN_POINT ( 'NONE',  ( -1.194742379459959869, -5.175423728813560054, 6.727584234649759409 ) ) ;
#16501 = CARTESIAN_POINT ( 'NONE',  ( 2.500000000000000000, 11.15000000000000036, 1.600000000000000089 ) ) ;
#16502 = PRESENTATION_LAYER_ASSIGNMENT (  '', '', ( #4377 ) ) ;
#16503 = EDGE_LOOP ( 'NONE', ( #8094, #18210, #6258, #3058 ) ) ;
#16504 = CARTESIAN_POINT ( 'NONE',  ( 2.135041058613650122, -0.7991276453871950514, 5.690123914223769397 ) ) ;
#16505 = VECTOR ( 'NONE', #15829, 1000.000000000000000 ) ;
#16506 = CARTESIAN_POINT ( 'NONE',  ( 0.000000000000000000, 0.000000000000000000, 5.100000000000000533 ) ) ;
#16507 = CARTESIAN_POINT ( 'NONE',  ( 2.351212046067109984, -0.9815930753335269099, 4.597298481426010497 ) ) ;
#16508 = CARTESIAN_POINT ( 'NONE',  ( -1.851400890972779045, -0.1868644067796610686, 6.601359968904141340 ) ) ;
#16509 = VECTOR ( 'NONE', #10665, 1000.000000000000000 ) ;
#16510 = EDGE_CURVE ( 'NONE', #4420, #10043, #3757, .T. ) ;
#16511 = CARTESIAN_POINT ( 'NONE',  ( 2.318251751302029984, -0.3667372881355940306, 4.294764266798990704 ) ) ;
#16512 = CARTESIAN_POINT ( 'NONE',  ( -1.713314936023349944, -0.5610169491525430763, 3.089913064446579760 ) ) ;
#16513 = EDGE_CURVE ( 'NONE', #8948, #5954, #9292, .T. ) ;
#16514 = CARTESIAN_POINT ( 'NONE',  ( -1.031876288691620625, -0.1690677966101698793, 7.145012538880312292 ) ) ;
#16515 = EDGE_LOOP ( 'NONE', ( #7314, #1429, #14707 ) ) ;
#16516 = ADVANCED_FACE ( 'NONE', ( #16246 ), #12269, .T. ) ;
#16517 = AXIS2_PLACEMENT_3D ( 'NONE', #9522, #8054, #14894 ) ;
#16518 = VECTOR ( 'NONE', #3240, 1000.000000000000000 ) ;
#16519 = LINE ( 'NONE', #9380, #1433 ) ;
#16520 = AXIS2_PLACEMENT_3D ( 'NONE', #14741, #17682, #668 ) ;
#16521 = CARTESIAN_POINT ( 'NONE',  ( -2.260890494820599450, -1.544352870612419881, 4.046455925041200885 ) ) ;
#16522 = SHAPE_REPRESENTATION_RELATIONSHIP ( 'NONE' , 'NONE' ,  #5932, #7745 ) ;
#16523 = CARTESIAN_POINT ( 'NONE',  ( 0.9150601050661639757, -5.430932203389830626, 6.868218666554230190 ) ) ;
#16524 = CARTESIAN_POINT ( 'NONE',  ( -2.524473153133541814, -4.987178660919110662, 3.881373716577405819 ) ) ;
#16525 = EDGE_LOOP ( 'NONE', ( #16116, #7133, #2610, #15279 ) ) ;
#16526 = AXIS2_PLACEMENT_3D ( 'NONE', #18190, #852, #17858 ) ;
#16527 = CARTESIAN_POINT ( 'NONE',  ( -1.899999999999999911, 2.000000000000000000, 1.600000000000000089 ) ) ;
#16528 = CARTESIAN_POINT ( 'NONE',  ( 2.255259958075439997, -3.896469987729530349, 5.372717034855999607 ) ) ;
#16529 = CARTESIAN_POINT ( 'NONE',  ( -2.573461662271331551, -4.847448931189385135, 5.348389362822530302 ) ) ;
#16530 = DIRECTION ( 'NONE',  ( 0.000000000000000000, -1.000000000000000000, 0.000000000000000000 ) ) ;
#16531 = LINE ( 'NONE', #9491, #3786 ) ;
#16532 = VECTOR ( 'NONE', #10914, 1000.000000000000000 ) ;
#16533 = CARTESIAN_POINT ( 'NONE',  ( -1.790316459643189972, -4.734848366107908824, 3.695177221627210074 ) ) ;
#16534 = CARTESIAN_POINT ( 'NONE',  ( -1.899999999999999911, 10.00000000000000000, 1.600000000000000089 ) ) ;
#16535 = LINE ( 'NONE', #10785, #856 ) ;
#16536 = VERTEX_POINT ( 'NONE', #4847 ) ;
#16537 = CARTESIAN_POINT ( 'NONE',  ( -1.399999999999999911, 6.400000000000000355, 7.700000000000000178 ) ) ;
#16538 = CARTESIAN_POINT ( 'NONE',  ( 1.800000000000000044, 11.29999999999999893, 7.649999999999999467 ) ) ;
#16539 = CARTESIAN_POINT ( 'NONE',  ( -1.449568901432419343, -0.2625000000000002331, 3.250431098567584165 ) ) ;
#16540 = EDGE_CURVE ( 'NONE', #16693, #4545, #2463, .T. ) ;
#16541 = CARTESIAN_POINT ( 'NONE',  ( -0.1749999999999999889, 6.799999999999999822, 1.600000000000000089 ) ) ;
#16542 = CARTESIAN_POINT ( 'NONE',  ( -0.8642983280852033490, -2.732055573315119723, 7.209203477813437289 ) ) ;
#16543 = CARTESIAN_POINT ( 'NONE',  ( 0.000000000000000000, 0.000000000000000000, 7.700000000000000178 ) ) ;
#16544 = LINE ( 'NONE', #14773, #10656 ) ;
#16545 = CARTESIAN_POINT ( 'NONE',  ( -3.503171016405825766E-15, -5.300000000000000711, 2.649999999999998579 ) ) ;
#16546 = ORIENTED_EDGE ( 'NONE', *, *, #14331, .T. ) ;
#16547 = LINE ( 'NONE', #13389, #14516 ) ;
#16548 = CARTESIAN_POINT ( 'NONE',  ( 2.293398556041700065, -5.364194915254239859, 4.171956209133470317 ) ) ;
#16549 = AXIS2_PLACEMENT_3D ( 'NONE', #13526, #12045, #11022 ) ;
#16550 = PLANE ( 'NONE',  #9061 ) ;
#16551 = EDGE_LOOP ( 'NONE', ( #11801, #2046, #4324, #15373, #14032, #1288, #9767, #4726 ) ) ;
#16552 = CARTESIAN_POINT ( 'NONE',  ( -2.353194804772640314, -5.524364406779660008, 4.731327187377240229 ) ) ;
#16553 = CARTESIAN_POINT ( 'NONE',  ( 1.722199153441390074, -0.5041426604022090086, 3.099360556065540173 ) ) ;
#16554 = FACE_OUTER_BOUND ( 'NONE', #16218, .T. ) ;
#16555 = FACE_OUTER_BOUND ( 'NONE', #8179, .T. ) ;
#16556 = CARTESIAN_POINT ( 'NONE',  ( -2.018065005288401270, -1.427911429170979352, 5.077247235985114848 ) ) ;
#16557 = PLANE ( 'NONE',  #2268 ) ;
#16558 = CARTESIAN_POINT ( 'NONE',  ( 0.6207106781186539912, 6.450000000000000178, 2.628553390593269423 ) ) ;
#16560 = VERTEX_POINT ( 'NONE', #16429 ) ;
#16559 = CARTESIAN_POINT ( 'NONE',  ( 2.594645788401200637, -2.611773255513701653, 5.257608218854235460 ) ) ;
#16561 = AXIS2_PLACEMENT_3D ( 'NONE', #3132, #3320, #11563 ) ;
#16562 = EDGE_CURVE ( 'NONE', #9239, #2742, #7916, .T. ) ;
#16563 = CARTESIAN_POINT ( 'NONE',  ( 0.009452039534070141164, -0.3001931771041043140, 2.350000000173209092 ) ) ;
#16564 = CARTESIAN_POINT ( 'NONE',  ( 2.345900685764729765, -0.3711864406779670222, 4.512231114381330066 ) ) ;
#16565 = CARTESIAN_POINT ( 'NONE',  ( 2.211317922628870392, -2.472043525783979678, 3.894507149290419967 ) ) ;
#16566 = CARTESIAN_POINT ( 'NONE',  ( 0.008535039157538009888, -5.014726856582200298, 2.281464080633750058 ) ) ;
#16567 = FACE_OUTER_BOUND ( 'NONE', #14511, .T. ) ;
#16568 = CARTESIAN_POINT ( 'NONE',  ( -0.08231150243516484333, -5.598516949152545941, 2.050000000000001155 ) ) ;
#16569 = VERTEX_POINT ( 'NONE', #3551 ) ;
#16570 = CARTESIAN_POINT ( 'NONE',  ( -0.5500000000000000444, 6.450000000000000178, 3.600000000000000089 ) ) ;
#16571 = EDGE_LOOP ( 'NONE', ( #6812, #4905, #15688, #11092 ) ) ;
#16572 = CARTESIAN_POINT ( 'NONE',  ( 1.112838723655039885, -5.126483050847459033, 6.773667561836209217 ) ) ;
#16573 = FACE_OUTER_BOUND ( 'NONE', #6422, .T. ) ;
#16574 = CARTESIAN_POINT ( 'NONE',  ( -0.005674314996646560166, -0.5399330878477630602, 2.472195840738689920 ) ) ;
#16575 = ADVANCED_FACE ( 'NONE', ( #2075 ), #10881, .F. ) ;
#16576 = ORIENTED_EDGE ( 'NONE', *, *, #2944, .F. ) ;
#16577 = AXIS2_PLACEMENT_3D ( 'NONE', #5903, #11629, #8946 ) ;
#16578 = CARTESIAN_POINT ( 'NONE',  ( 2.342931736853870017, -4.102223705964150646, 4.477701633099130163 ) ) ;
#16579 = LINE ( 'NONE', #5178, #5865 ) ;
#16580 = CARTESIAN_POINT ( 'NONE',  ( 1.112838723655040107, -5.426483050847459744, 6.773667561836210105 ) ) ;
#16581 = CARTESIAN_POINT ( 'NONE',  ( -0.1749999999999999889, 4.299999999999999822, 1.600000000000000089 ) ) ;
#16582 = CARTESIAN_POINT ( 'NONE',  ( -1.948278411993560111, -3.193980462720909852, 6.020210936496040333 ) ) ;
#16583 = DIRECTION ( 'NONE',  ( 1.000000000000000000, 5.782411586589356455E-15, 3.614007241618347587E-15 ) ) ;
#16584 = DIRECTION ( 'NONE',  ( 0.000000000000000000, 0.000000000000000000, 1.000000000000000000 ) ) ;
#16585 = VECTOR ( 'NONE', #7835, 1000.000000000000000 ) ;
#16586 = CARTESIAN_POINT ( 'NONE',  ( -0.9290506585603975909, -0.5829339996946386604, 2.210445150547709403 ) ) ;
#16587 = ORIENTED_EDGE ( 'NONE', *, *, #16387, .T. ) ;
#16588 = LINE ( 'NONE', #848, #3971 ) ;
#16589 = SURFACE_STYLE_USAGE ( .BOTH. , #2338 ) ;
#16590 = ORIENTED_EDGE ( 'NONE', *, *, #2569, .F. ) ;
#16591 = EDGE_LOOP ( 'NONE', ( #10525, #14142, #14549, #13585 ) ) ;
#16592 = EDGE_CURVE ( 'NONE', #5474, #1639, #3641, .T. ) ;
#16593 = PRODUCT_DEFINITION_CONTEXT ( 'detailed design', #7798, 'design' ) ;
#16594 =( BOUNDED_SURFACE ( )  B_SPLINE_SURFACE ( 3, 3, ( 
 ( #11861, #10278, #4891, #17206, #4529, #9056, #4799, #9155, #8804, #17479, #14456, #7687, #464, #7422, #13063, #3408, #383, #8890, #14541, #1938, #1857, #17560, #11771, #7504, #14713, #7777, #2032, #6023, #3331, #11668, #13151, #14623, #13332, #15947, #6107, #8976, #17398, #4716, #645, #10365, #7589, #6283, #11943, #16203, #3512, #14818, #5379, #2427, #6762, #12038, #17661, #9254, #3605, #3794, #16479, #12139, #8249, #12320, #12412, #17759, #14913, #6662, #5184, #16667, #15198, #18034, #2222, #1025, #5090, #5001, #6372, #17939, #15113, #11018, #7869, #5284, #737, #7976, #10742, #16390, #13624, #13520, #838, #3973, #6480, #1117, #3692, #9625, #9340, #15010, #10652, #15285, #16299, #2327, #935, #6573, #12227, #2597, #10935, #17846, #10833, #9451, #8072, #13712, #16582, #3888, #9542, #2506, #8153, #13792, #17016, #13891, #5464, #11102, #18115, #14168, #1206, #15472, #1487, #3049, #1379, #2780, #16749, #4333, #5557, #12863, #15663, #2869, #1575, #7045, #10000, #6854, #12500, #12781, #7221, #14061, #175, #17108, #5822, #12585, #11473, #7144, #16932, #4063, #9720, #4242, #15743, #4432, #5652, #8424, #8519, #9904, #15389, #10091, #12688, #2687, #18200, #15561, #95, #11296, #2972, #8340, #6938, #5738, #13973, #10, #1294, #11383, #8613, #14256, #11202, #16847, #4158, #9814, #13217, #7666, #4592, #4873, #1756, #11645, #15824, #3229, #539, #8961, #2011, #14693, #16096, #17272 ),
 ( #278, #10519, #1921, #1844, #17190, #14433, #13311, #7404, #3127, #16016, #11841, #10433, #7487, #13043, #13135, #6185, #11925, #17464, #4783, #10164, #8874, #3391, #16182, #8691, #9036, #14605, #8779, #364, #6002, #6089, #10350, #11742, #17376, #7305, #12953, #10251, #15918, #14523, #7570, #5919, #627, #11559, #6266, #447, #17543, #4697, #14337, #3317, #1656, #4514, #916, #12121, #6455, #9320, #5160, #12016, #10810, #10915, #17740, #6639, #717, #16457, #4974, #2106, #7956, #5068, #3672, #13402, #10720, #6554, #815, #3582, #12207, #9229, #1002, #3868, #3488, #3770, #17823, #16559, #9133, #9430, #14792, #13694, #16368, #6351, #10629, #15094, #16277, #14990, #2303, #2405, #13601, #5261, #8052, #12296, #17916, #7757, #17636, #14891, #2204, #7848, #13498, #10402, #10485, #14495, #7460, #4751, #419, #3287, #14754, #8848, #6055, #16238, #4840, #11704, #7722, #13182, #6318, #3360, #13366, #13014, #337, #10218, #4562, #16062, #17433, #13105, #9191, #13278, #679, #17336, #15884, #7632, #6149, #17592, #16144, #11980, #3195, #1970, #4666, #5972, #7375, #596, #9003, #4930, #1817, #6235, #1723, #8930, #10321, #15984, #14575, #1891, #7538, #10585, #498, #2068, #11808, #3544, #14656, #11895, #11616, #17243, #17514, #3445, #9093, #10686, #2169, #2534, #13559, #16420, #9572, #3634, #875, #11048, #17979, #6514, #8184, #8011, #1153, #16524, #13834, #7810, #13457, #5030, #17698, #17879 ),
 ( #16329, #2454, #965, #12448, #10970, #6800, #9285, #15143, #7911, #774, #6406, #8101, #10874, #18065, #14948, #1058, #14853, #3726, #12171, #17788, #9387, #2258, #5125, #5408, #10775, #15230, #15055, #16697, #2361, #13655, #12077, #4006, #6603, #12261, #5216, #3834, #9482, #13740, #6698, #12356, #5324, #16615, #3916, #5477, #12600, #9741, #12707, #18220, #6953, #2795, #16949, #13909, #15575, #5392, #5575, #9638, #15304, #2887, #11117, #8267, #1399, #16864, #4172, #1223, #8439, #24, #14073, #16764, #5669, #15404, #2709, #11311, #14187, #1503, #6343, #10712, #7235, #708, #14981, #9218, #1771, #12879, #15756, #12007, #3063, #4526, #10178, #3479, #15842, #804, #13059, #3140, #2097, #3664, #17626, #192, #17287, #8707, #8799, #15941, #16268, #1675, #12969, #10270, #4612, #293, #5837, #4965, #6445, #5931, #14349, #13394, #11662, #5061, #3571, #12112, #7324, #7748, #11571, #11489, #17121, #10620, #9125, #17732, #17202, #14882, #4445, #14450, #7418, #378, #6018, #14781, #2196, #16358, #7840, #13487, #9312, #10105, #2396, #17909, #6546, #8314, #7947, #16448, #10908, #3759, #13593, #13952, #1180, #13762, #18173, #6631, #2661, #15086, #2482, #12288, #2560, #8126, #9513, #18006, #6828, #9422, #18090, #16819, #15172, #6913, #5152, #5437, #8045, #12199, #9599, #1084, #12386, #17815, #6731, #8215, #3860, #994, #13863, #5251, #1269, #9788, #2293, #11078, #12472, #5524, #908, #16721 ),
 ( #13686, #16553, #5350, #10994, #4032, #9687, #12561, #11169, #15359, #16642, #3946, #15255, #4131, #10802, #2759, #12753, #7008, #17246, #14313, #8584, #5625, #2839, #3104, #8487, #9879, #4406, #251, #17167, #14229, #14134, #1549, #1634, #339, #12924, #5891, #16910, #9970, #7280, #4565, #1353, #10064, #15635, #7196, #12659, #2943, #3021, #16993, #1459, #11533, #7114, #14400, #15450, #8401, #4486, #10140, #5975, #14038, #15796, #18281, #8751, #12837, #11268, #4219, #1728, #15538, #68, #5714, #11441, #11360, #7379, #150, #4306, #15718, #11618, #13017, #5797, #17078, #6057, #500, #599, #681, #4670, #15986, #13281, #8932, #11811, #4934, #17338, #14579, #6410, #13369, #1895, #16242, #3363, #14857, #11897, #3547, #3199, #8851, #421, #13108, #6238, #7635, #3289, #17702, #3447, #9194, #7540, #11706, #16147, #14658, #7814, #6320, #2173, #10325, #10488, #13184, #14497, #15886, #9096, #17516, #13460, #6152, #14758, #10220, #17436, #4753, #10404, #16064, #9006, #1972, #777, #4842, #10588, #2070, #12082, #7725, #11983, #1819, #7462, #17596, #880, #13658, #6517, #10689, #11052, #3921, #16528, #2640, #9391, #5413, #17792, #5220, #15059, #5328, #10877, #12264, #2458, #9575, #12174, #2537, #1247, #17882, #9661, #7914, #8187, #5128, #3838, #15333, #6702, #16700, #16333, #3637, #13564, #10778, #8104, #13743, #16424, #12537, #16619, #4009, #3729, #2366, #10973, #9486, #8291, #1157, #13930 ),
 ( #1061, #6890, #8016, #15233, #5033, #15147, #969, #6606, #12360, #17982, #13837, #9289, #6804, #14951, #12451, #2261, #18068, #4850, #11817, #13574, #13191, #3369, #16154, #9012, #508, #888, #6421, #690, #5135, #11902, #7923, #1979, #7731, #17521, #7822, #13375, #14764, #4943, #12091, #14664, #5040, #3738, #2077, #12180, #10409, #10696, #7641, #17441, #14864, #6326, #17606, #4759, #11990, #13467, #9104, #6243, #785, #10495, #6524, #15067, #7545, #16339, #17709, #10786, #6161, #3643, #16071, #9294, #10596, #13286, #604, #14960, #3454, #16248, #3553, #9200, #2179, #17798, #2269, #16431, #9399, #17129, #14194, #2375, #12715, #16776, #11227, #11321, #11405, #15413, #8362, #5677, #1314, #4180, #15684, #9748, #6961, #4454, #5763, #12610, #8634, #1512, #8024, #32, #4089, #16872, #16957, #17037, #2717, #13995, #4265, #18232, #9839, #2994, #5583, #15493, #10112, #4363, #2802, #14279, #14081, #7246, #9924, #1602, #13664, #976, #10884, #5229, #15586, #2899, #8447, #6613, #7165, #12886, #1411, #7073, #8547, #12803, #203, #10025, #5848, #117, #11498, #12270, #17890, #3071, #16033, #11774, #7689, #11577, #1940, #15764, #4622, #14459, #8808, #10282, #17209, #4532, #647, #10184, #16113, #15849, #2034, #3151, #13066, #1683, #3410, #8715, #1778, #6026, #7426, #14359, #9059, #14625, #8894, #13335, #386, #14716, #11671, #15950, #17294, #3333, #3250, #14543, #13152, #7592, #1859, #13243 ),
 ( #7333, #4718, #7506, #466, #12978, #6110, #8978, #17400, #10368, #564, #6208, #6285, #4893, #300, #11864, #17481, #11945, #5939, #4801, #10452, #17562, #5092, #16206, #739, #15115, #6374, #7871, #13524, #6575, #842, #3890, #16392, #6482, #5187, #6766, #12229, #16482, #2331, #6665, #12041, #3608, #2429, #9544, #15012, #3514, #9342, #12141, #10937, #2508, #9157, #17664, #1120, #8074, #15201, #17761, #12414, #9257, #10744, #5003, #3695, #13714, #10835, #8155, #13796, #17942, #7978, #13626, #937, #18036, #10544, #14820, #17848, #2135, #7778, #3798, #9454, #10654, #16301, #13425, #14915, #2224, #1027, #12322, #5288, #4160, #16751, #9816, #9906, #8615, #2872, #8521, #6856, #18203, #15563, #12865, #5381, #14171, #5655, #18117, #15391, #4066, #2783, #7048, #8426, #14063, #3975, #9627, #8342, #2689, #11104, #16934, #15288, #4244, #2602, #8253, #16851, #1489, #11020, #13893, #1208, #12502, #11298, #16670, #6940, #7146, #5466, #11206, #12587, #9725, #12784, #13975, #4336, #97, #12692, #11385, #15474, #5740, #1296, #5560, #17018, #10002, #1381, #15666, #14258, #2974, #12, #1579, #7223, #3232, #178, #4435, #8876, #7670, #5824, #10253, #13046, #13137, #14526, #15745, #11475, #366, #10093, #4516, #3051, #16018, #3319, #1659, #6004, #4700, #8696, #14339, #10352, #449, #12955, #10167, #11561, #15921, #1846, #7489, #6091, #7307, #282, #3129, #15828, #5921, #11747, #17192, #17379 ),
 ( #8782, #14436, #11648, #1759, #17274, #4596, #8963, #14608, #1923, #13219, #8637, #1688, #9932, #1784, #9141, #17642, #12125, #4979, #14801, #9524, #2409, #14993, #1095, #7852, #3872, #16283, #3677, #13503, #3776, #9324, #10726, #920, #8056, #10634, #1009, #18015, #16372, #8139, #6356, #6645, #3588, #7763, #10814, #2311, #13606, #721, #7961, #9436, #5075, #2208, #15099, #821, #2491, #3494, #2111, #12300, #13698, #6744, #13408, #17921, #12021, #5267, #6558, #9233, #14896, #10920, #6461, #17744, #12213, #17829, #5163, #15183, #16461, #16565, #13774, #5362, #12396, #16652, #8410, #12482, #6922, #7022, #7127, #11088, #4046, #1362, #15368, #18182, #11367, #5447, #2671, #12845, #1468, #8324, #4316, #9797, #2953, #9887, #5805, #76, #11184, #3958, #6838, #2850, #18100, #13959, #1279, #12669, #12569, #15646, #4139, #5536, #11277, #159, #8497, #9608, #14046, #16729, #16829, #10040, #12763, #9701, #15457, #5634, #2765, #16918, #17000, #4227, #14147, #15269, #5721, #8593, #14240, #1558, #7203, #2574, #8227, #13874, #1189, #1641, #14321, #14507, #8859, #4495, #611, #4681, #4765, #10150, #7288, #17352, #15900, #9019, #7551, #10417, #12934, #11719, #15805, #10075, #17089, #10335, #7471, #3375, #263, #15998, #11454, #348, #3111, #8763, #5987, #5900, #11542, #14669, #17175, #11824, #14413, #16078, #1738, #7388, #15727, #17447, #4416, #13025, #11627, #17257, #3032, #1988, #3301, #4573 ) ),
 .UNSPECIFIED., .T., .F., .F. ) 
 B_SPLINE_SURFACE_WITH_KNOTS ( ( 4, 3, 4 ),
 ( 4, 1, 1, 1, 1, 1, 1, 1, 1, 1, 1, 1, 1, 1, 1, 1, 1, 1, 1, 1, 1, 1, 1, 1, 1, 1, 1, 1, 1, 1, 1, 1, 1, 1, 1, 1, 1, 1, 1, 1, 1, 1, 1, 1, 1, 1, 1, 1, 1, 1, 1, 1, 1, 1, 1, 1, 1, 1, 1, 1, 1, 1, 1, 1, 1, 1, 1, 1, 1, 1, 1, 1, 1, 1, 1, 1, 1, 1, 1, 1, 1, 1, 1, 1, 1, 1, 1, 1, 1, 1, 1, 1, 1, 1, 1, 1, 1, 1, 1, 1, 1, 1, 1, 1, 1, 1, 1, 1, 1, 1, 1, 1, 1, 1, 1, 1, 1, 1, 1, 1, 1, 1, 1, 1, 1, 1, 1, 1, 1, 1, 1, 1, 1, 1, 1, 1, 1, 1, 1, 1, 1, 1, 1, 1, 1, 1, 1, 1, 1, 1, 1, 1, 1, 1, 1, 1, 1, 1, 1, 1, 1, 1, 1, 1, 1, 1, 1, 1, 1, 1, 1, 1, 1, 1, 1, 1, 1, 1, 1, 1, 1, 1, 1, 1, 1, 4 ),
 ( 0.000000000000000000, 3.141592653589790007, 6.283185307179590673 ),
 ( 0.7853981633974479459, 0.8787968639095770085, 0.9721955644217059600, 1.065594264933839908, 1.158992965445959866, 1.252391665958090039, 1.345790366470219990, 1.439189066982349940, 1.532587767494480113, 1.625986468006610064, 1.719385168518740015, 1.812783869030869965, 1.906182569543000138, 1.999581270055129867, 2.092979970567249826, 2.186378671079379998, 2.279777371591510171, 2.373176072103639900, 2.466574772615769628, 2.559973473127900245, 2.653372173640029974, 2.746770874152160147, 2.840169574664289875, 2.933568275176409834, 3.026966975688540007, 3.120365676200670180, 3.213764376712799908, 3.307163077224930081, 3.400561777737059810, 3.493960478249190427, 3.587359178761320155, 3.680757879273439670, 3.774156579785570287, 3.867555280297700016, 3.960953980809830188, 4.054352681321960361, 4.147751381834090090, 4.241150082346219818, 4.334548782858350435, 4.427947483370480164, 4.521346183882600123, 4.614744884394729851, 4.708143584906859580, 4.801542285418989309, 4.894940985931119926, 4.988339686443250542, 5.081738386955380271, 5.175137087467510000, 5.268535787979639728, 5.361934488491760575, 5.455333189003890304, 5.548731889516020033, 5.642130590028149761, 5.735529290540279490, 5.828927991052410107, 5.922326691564539836, 6.015725392076670452, 6.109124092588789523, 6.202522793100920140, 6.295921493613049869, 6.389320194125180485, 6.482718894637310214, 6.576117595149439943, 6.669516295661569671, 6.762914996173699400, 6.856313696685830017, 6.949712397197949976, 7.043111097710079704, 7.136509798222209433, 7.229908498734340050, 7.323307199246470667, 7.416705899758600395, 7.510104600270730124, 7.603503300782859853, 7.696902001294989581, 7.790300701807110428, 7.883699402319240157, 7.977098102831369886, 8.070496803343500503, 8.163895503855631119, 8.257294204367759960, 8.350692904879890577, 8.444091605392019417, 8.537490305904139376, 8.630889006416269993, 8.724287706928398833, 8.817686407440529450, 8.911085107952660067, 9.004483808464788908, 9.097882508976921301, 9.191281209489050141, 9.284679910001178982, 9.378078610513298941, 9.471477311025429557, 9.564876011537560174, 9.658274712049690791, 9.751673412561819632, 9.845072113073950248, 9.938470813586080865, 10.03186951409819905, 10.12526821461029947, 10.21866691512249936, 10.31206561563459978, 10.40546431614669842, 10.49886301665890009, 10.59226171717100051, 10.68566041768310093, 10.77905911819519957, 10.87245781870739947, 10.96585651921949989, 11.05925521973160031, 11.15265392024380020, 11.24605262075590062, 11.33945132126800104, 11.43285002178009968, 11.52624872229229958, 11.61964742280439999, 11.71304612331650041, 11.80644482382869853, 11.89984352434079895, 11.99324222485290115, 12.08664092536500156, 12.18003962587719968, 12.27343832638930010, 12.36683702690140052, 12.46023572741360042, 12.55363442792569906, 12.64703312843779948, 12.74043182894989990, 12.83383052946209979, 12.92722922997419843, 13.02062793048630063, 13.11402663099850052, 13.20742533151059916, 13.30082403202269958, 13.39422273253480000, 13.48762143304700167, 13.58102013355910032, 13.67441883407120073, 13.76781753458340063, 13.86121623509549927, 13.95461493560759969, 14.04801363611970011, 14.14141233663190000, 14.23481103714399865, 14.32820973765609907, 14.42160843816829896, 14.51500713868040116, 14.60840583919249980, 14.70180453970460022, 14.79520324021680011, 14.88860194072889875, 14.98200064124100095, 15.07539934175320084, 15.16879804226530126, 15.26219674277739990, 15.35559544328959980, 15.44899414380170022, 15.54239284431380064, 15.63579154482589928, 15.72919024533809917, 15.82258894585019959, 15.91598764636230001, 16.00938634687449991, 16.10278504738660033, 16.19618374789869719, 16.28958244841080116, 16.38298114892299751, 16.47637984943510148, 16.56977854994720190, 16.66317725045940179, 16.75657595097149866, 16.84997465148359908, 16.94337335199570305, 17.03677205250789939, 17.13017075301999981, 17.22356945353210023, 17.31696815404430012, 17.41036685455640054, 17.50376555506850096, 17.59716425558059782, 17.69056295609280127, 17.78396165660489814, 17.87736035711699856, 17.97075905762920200, 18.06415775814129887 ),
 .UNSPECIFIED. ) 
 GEOMETRIC_REPRESENTATION_ITEM ( )  RATIONAL_B_SPLINE_SURFACE ( (
 ( 1.000000000000000000, 1.000000000000000000, 1.000000000000000000, 1.000000000000000000, 1.000000000000000000, 1.000000000000000000, 1.000000000000000000, 1.000000000000000000, 1.000000000000000000, 1.000000000000000000, 1.000000000000000000, 1.000000000000000000, 1.000000000000000000, 1.000000000000000000, 1.000000000000000000, 1.000000000000000000, 1.000000000000000000, 1.000000000000000000, 1.000000000000000000, 1.000000000000000000, 1.000000000000000000, 1.000000000000000000, 1.000000000000000000, 1.000000000000000000, 1.000000000000000000, 1.000000000000000000, 1.000000000000000000, 1.000000000000000000, 1.000000000000000000, 1.000000000000000000, 1.000000000000000000, 1.000000000000000000, 1.000000000000000000, 1.000000000000000000, 1.000000000000000000, 1.000000000000000000, 1.000000000000000000, 1.000000000000000000, 1.000000000000000000, 1.000000000000000000, 1.000000000000000000, 1.000000000000000000, 1.000000000000000000, 1.000000000000000000, 1.000000000000000000, 1.000000000000000000, 1.000000000000000000, 1.000000000000000000, 1.000000000000000000, 1.000000000000000000, 1.000000000000000000, 1.000000000000000000, 1.000000000000000000, 1.000000000000000000, 1.000000000000000000, 1.000000000000000000, 1.000000000000000000, 1.000000000000000000, 1.000000000000000000, 1.000000000000000000, 1.000000000000000000, 1.000000000000000000, 1.000000000000000000, 1.000000000000000000, 1.000000000000000000, 1.000000000000000000, 1.000000000000000000, 1.000000000000000000, 1.000000000000000000, 1.000000000000000000, 1.000000000000000000, 1.000000000000000000, 1.000000000000000000, 1.000000000000000000, 1.000000000000000000, 1.000000000000000000, 1.000000000000000000, 1.000000000000000000, 1.000000000000000000, 1.000000000000000000, 1.000000000000000000, 1.000000000000000000, 1.000000000000000000, 1.000000000000000000, 1.000000000000000000, 1.000000000000000000, 1.000000000000000000, 1.000000000000000000, 1.000000000000000000, 1.000000000000000000, 1.000000000000000000, 1.000000000000000000, 1.000000000000000000, 1.000000000000000000, 1.000000000000000000, 1.000000000000000000, 1.000000000000000000, 1.000000000000000000, 1.000000000000000000, 1.000000000000000000, 1.000000000000000000, 1.000000000000000000, 1.000000000000000000, 1.000000000000000000, 1.000000000000000000, 1.000000000000000000, 1.000000000000000000, 1.000000000000000000, 1.000000000000000000, 1.000000000000000000, 1.000000000000000000, 1.000000000000000000, 1.000000000000000000, 1.000000000000000000, 1.000000000000000000, 1.000000000000000000, 1.000000000000000000, 1.000000000000000000, 1.000000000000000000, 1.000000000000000000, 1.000000000000000000, 1.000000000000000000, 1.000000000000000000, 1.000000000000000000, 1.000000000000000000, 1.000000000000000000, 1.000000000000000000, 1.000000000000000000, 1.000000000000000000, 1.000000000000000000, 1.000000000000000000, 1.000000000000000000, 1.000000000000000000, 1.000000000000000000, 1.000000000000000000, 1.000000000000000000, 1.000000000000000000, 1.000000000000000000, 1.000000000000000000, 1.000000000000000000, 1.000000000000000000, 1.000000000000000000, 1.000000000000000000, 1.000000000000000000, 1.000000000000000000, 1.000000000000000000, 1.000000000000000000, 1.000000000000000000, 1.000000000000000000, 1.000000000000000000, 1.000000000000000000, 1.000000000000000000, 1.000000000000000000, 1.000000000000000000, 1.000000000000000000, 1.000000000000000000, 1.000000000000000000, 1.000000000000000000, 1.000000000000000000, 1.000000000000000000, 1.000000000000000000, 1.000000000000000000, 1.000000000000000000, 1.000000000000000000, 1.000000000000000000, 1.000000000000000000, 1.000000000000000000, 1.000000000000000000, 1.000000000000000000, 1.000000000000000000, 1.000000000000000000, 1.000000000000000000, 1.000000000000000000, 1.000000000000000000, 1.000000000000000000, 1.000000000000000000, 1.000000000000000000, 1.000000000000000000, 1.000000000000000000, 1.000000000000000000, 1.000000000000000000, 1.000000000000000000, 1.000000000000000000, 1.000000000000000000, 1.000000000000000000, 1.000000000000000000, 1.000000000000000000, 1.000000000000000000),
 ( 0.3333333333333329818, 0.3333333333333329818, 0.3333333333333329818, 0.3333333333333329818, 0.3333333333333329818, 0.3333333333333329818, 0.3333333333333329818, 0.3333333333333329818, 0.3333333333333329818, 0.3333333333333329818, 0.3333333333333329818, 0.3333333333333329818, 0.3333333333333329818, 0.3333333333333329818, 0.3333333333333329818, 0.3333333333333329818, 0.3333333333333329818, 0.3333333333333329818, 0.3333333333333329818, 0.3333333333333329818, 0.3333333333333329818, 0.3333333333333329818, 0.3333333333333329818, 0.3333333333333329818, 0.3333333333333329818, 0.3333333333333329818, 0.3333333333333329818, 0.3333333333333329818, 0.3333333333333329818, 0.3333333333333329818, 0.3333333333333329818, 0.3333333333333329818, 0.3333333333333329818, 0.3333333333333329818, 0.3333333333333329818, 0.3333333333333329818, 0.3333333333333329818, 0.3333333333333329818, 0.3333333333333329818, 0.3333333333333329818, 0.3333333333333329818, 0.3333333333333329818, 0.3333333333333329818, 0.3333333333333329818, 0.3333333333333329818, 0.3333333333333329818, 0.3333333333333329818, 0.3333333333333329818, 0.3333333333333329818, 0.3333333333333329818, 0.3333333333333329818, 0.3333333333333329818, 0.3333333333333329818, 0.3333333333333329818, 0.3333333333333329818, 0.3333333333333329818, 0.3333333333333329818, 0.3333333333333329818, 0.3333333333333329818, 0.3333333333333329818, 0.3333333333333329818, 0.3333333333333329818, 0.3333333333333329818, 0.3333333333333329818, 0.3333333333333329818, 0.3333333333333329818, 0.3333333333333329818, 0.3333333333333329818, 0.3333333333333329818, 0.3333333333333329818, 0.3333333333333329818, 0.3333333333333329818, 0.3333333333333329818, 0.3333333333333329818, 0.3333333333333329818, 0.3333333333333329818, 0.3333333333333329818, 0.3333333333333329818, 0.3333333333333329818, 0.3333333333333329818, 0.3333333333333329818, 0.3333333333333329818, 0.3333333333333329818, 0.3333333333333329818, 0.3333333333333329818, 0.3333333333333329818, 0.3333333333333329818, 0.3333333333333329818, 0.3333333333333329818, 0.3333333333333329818, 0.3333333333333329818, 0.3333333333333329818, 0.3333333333333329818, 0.3333333333333329818, 0.3333333333333329818, 0.3333333333333329818, 0.3333333333333329818, 0.3333333333333329818, 0.3333333333333329818, 0.3333333333333329818, 0.3333333333333329818, 0.3333333333333329818, 0.3333333333333329818, 0.3333333333333329818, 0.3333333333333329818, 0.3333333333333329818, 0.3333333333333329818, 0.3333333333333329818, 0.3333333333333329818, 0.3333333333333329818, 0.3333333333333329818, 0.3333333333333329818, 0.3333333333333329818, 0.3333333333333329818, 0.3333333333333329818, 0.3333333333333329818, 0.3333333333333329818, 0.3333333333333329818, 0.3333333333333329818, 0.3333333333333329818, 0.3333333333333329818, 0.3333333333333329818, 0.3333333333333329818, 0.3333333333333329818, 0.3333333333333329818, 0.3333333333333329818, 0.3333333333333329818, 0.3333333333333329818, 0.3333333333333329818, 0.3333333333333329818, 0.3333333333333329818, 0.3333333333333329818, 0.3333333333333329818, 0.3333333333333329818, 0.3333333333333329818, 0.3333333333333329818, 0.3333333333333329818, 0.3333333333333329818, 0.3333333333333329818, 0.3333333333333329818, 0.3333333333333329818, 0.3333333333333329818, 0.3333333333333329818, 0.3333333333333329818, 0.3333333333333329818, 0.3333333333333329818, 0.3333333333333329818, 0.3333333333333329818, 0.3333333333333329818, 0.3333333333333329818, 0.3333333333333329818, 0.3333333333333329818, 0.3333333333333329818, 0.3333333333333329818, 0.3333333333333329818, 0.3333333333333329818, 0.3333333333333329818, 0.3333333333333329818, 0.3333333333333329818, 0.3333333333333329818, 0.3333333333333329818, 0.3333333333333329818, 0.3333333333333329818, 0.3333333333333329818, 0.3333333333333329818, 0.3333333333333329818, 0.3333333333333329818, 0.3333333333333329818, 0.3333333333333329818, 0.3333333333333329818, 0.3333333333333329818, 0.3333333333333329818, 0.3333333333333329818, 0.3333333333333329818, 0.3333333333333329818, 0.3333333333333329818, 0.3333333333333329818, 0.3333333333333329818, 0.3333333333333329818, 0.3333333333333329818, 0.3333333333333329818, 0.3333333333333329818, 0.3333333333333329818, 0.3333333333333329818, 0.3333333333333329818, 0.3333333333333329818, 0.3333333333333329818, 0.3333333333333329818),
 ( 0.3333333333333329818, 0.3333333333333329818, 0.3333333333333329818, 0.3333333333333329818, 0.3333333333333329818, 0.3333333333333329818, 0.3333333333333329818, 0.3333333333333329818, 0.3333333333333329818, 0.3333333333333329818, 0.3333333333333329818, 0.3333333333333329818, 0.3333333333333329818, 0.3333333333333329818, 0.3333333333333329818, 0.3333333333333329818, 0.3333333333333329818, 0.3333333333333329818, 0.3333333333333329818, 0.3333333333333329818, 0.3333333333333329818, 0.3333333333333329818, 0.3333333333333329818, 0.3333333333333329818, 0.3333333333333329818, 0.3333333333333329818, 0.3333333333333329818, 0.3333333333333329818, 0.3333333333333329818, 0.3333333333333329818, 0.3333333333333329818, 0.3333333333333329818, 0.3333333333333329818, 0.3333333333333329818, 0.3333333333333329818, 0.3333333333333329818, 0.3333333333333329818, 0.3333333333333329818, 0.3333333333333329818, 0.3333333333333329818, 0.3333333333333329818, 0.3333333333333329818, 0.3333333333333329818, 0.3333333333333329818, 0.3333333333333329818, 0.3333333333333329818, 0.3333333333333329818, 0.3333333333333329818, 0.3333333333333329818, 0.3333333333333329818, 0.3333333333333329818, 0.3333333333333329818, 0.3333333333333329818, 0.3333333333333329818, 0.3333333333333329818, 0.3333333333333329818, 0.3333333333333329818, 0.3333333333333329818, 0.3333333333333329818, 0.3333333333333329818, 0.3333333333333329818, 0.3333333333333329818, 0.3333333333333329818, 0.3333333333333329818, 0.3333333333333329818, 0.3333333333333329818, 0.3333333333333329818, 0.3333333333333329818, 0.3333333333333329818, 0.3333333333333329818, 0.3333333333333329818, 0.3333333333333329818, 0.3333333333333329818, 0.3333333333333329818, 0.3333333333333329818, 0.3333333333333329818, 0.3333333333333329818, 0.3333333333333329818, 0.3333333333333329818, 0.3333333333333329818, 0.3333333333333329818, 0.3333333333333329818, 0.3333333333333329818, 0.3333333333333329818, 0.3333333333333329818, 0.3333333333333329818, 0.3333333333333329818, 0.3333333333333329818, 0.3333333333333329818, 0.3333333333333329818, 0.3333333333333329818, 0.3333333333333329818, 0.3333333333333329818, 0.3333333333333329818, 0.3333333333333329818, 0.3333333333333329818, 0.3333333333333329818, 0.3333333333333329818, 0.3333333333333329818, 0.3333333333333329818, 0.3333333333333329818, 0.3333333333333329818, 0.3333333333333329818, 0.3333333333333329818, 0.3333333333333329818, 0.3333333333333329818, 0.3333333333333329818, 0.3333333333333329818, 0.3333333333333329818, 0.3333333333333329818, 0.3333333333333329818, 0.3333333333333329818, 0.3333333333333329818, 0.3333333333333329818, 0.3333333333333329818, 0.3333333333333329818, 0.3333333333333329818, 0.3333333333333329818, 0.3333333333333329818, 0.3333333333333329818, 0.3333333333333329818, 0.3333333333333329818, 0.3333333333333329818, 0.3333333333333329818, 0.3333333333333329818, 0.3333333333333329818, 0.3333333333333329818, 0.3333333333333329818, 0.3333333333333329818, 0.3333333333333329818, 0.3333333333333329818, 0.3333333333333329818, 0.3333333333333329818, 0.3333333333333329818, 0.3333333333333329818, 0.3333333333333329818, 0.3333333333333329818, 0.3333333333333329818, 0.3333333333333329818, 0.3333333333333329818, 0.3333333333333329818, 0.3333333333333329818, 0.3333333333333329818, 0.3333333333333329818, 0.3333333333333329818, 0.3333333333333329818, 0.3333333333333329818, 0.3333333333333329818, 0.3333333333333329818, 0.3333333333333329818, 0.3333333333333329818, 0.3333333333333329818, 0.3333333333333329818, 0.3333333333333329818, 0.3333333333333329818, 0.3333333333333329818, 0.3333333333333329818, 0.3333333333333329818, 0.3333333333333329818, 0.3333333333333329818, 0.3333333333333329818, 0.3333333333333329818, 0.3333333333333329818, 0.3333333333333329818, 0.3333333333333329818, 0.3333333333333329818, 0.3333333333333329818, 0.3333333333333329818, 0.3333333333333329818, 0.3333333333333329818, 0.3333333333333329818, 0.3333333333333329818, 0.3333333333333329818, 0.3333333333333329818, 0.3333333333333329818, 0.3333333333333329818, 0.3333333333333329818, 0.3333333333333329818, 0.3333333333333329818, 0.3333333333333329818, 0.3333333333333329818, 0.3333333333333329818, 0.3333333333333329818, 0.3333333333333329818, 0.3333333333333329818, 0.3333333333333329818, 0.3333333333333329818, 0.3333333333333329818),
 ( 1.000000000000000000, 1.000000000000000000, 1.000000000000000000, 1.000000000000000000, 1.000000000000000000, 1.000000000000000000, 1.000000000000000000, 1.000000000000000000, 1.000000000000000000, 1.000000000000000000, 1.000000000000000000, 1.000000000000000000, 1.000000000000000000, 1.000000000000000000, 1.000000000000000000, 1.000000000000000000, 1.000000000000000000, 1.000000000000000000, 1.000000000000000000, 1.000000000000000000, 1.000000000000000000, 1.000000000000000000, 1.000000000000000000, 1.000000000000000000, 1.000000000000000000, 1.000000000000000000, 1.000000000000000000, 1.000000000000000000, 1.000000000000000000, 1.000000000000000000, 1.000000000000000000, 1.000000000000000000, 1.000000000000000000, 1.000000000000000000, 1.000000000000000000, 1.000000000000000000, 1.000000000000000000, 1.000000000000000000, 1.000000000000000000, 1.000000000000000000, 1.000000000000000000, 1.000000000000000000, 1.000000000000000000, 1.000000000000000000, 1.000000000000000000, 1.000000000000000000, 1.000000000000000000, 1.000000000000000000, 1.000000000000000000, 1.000000000000000000, 1.000000000000000000, 1.000000000000000000, 1.000000000000000000, 1.000000000000000000, 1.000000000000000000, 1.000000000000000000, 1.000000000000000000, 1.000000000000000000, 1.000000000000000000, 1.000000000000000000, 1.000000000000000000, 1.000000000000000000, 1.000000000000000000, 1.000000000000000000, 1.000000000000000000, 1.000000000000000000, 1.000000000000000000, 1.000000000000000000, 1.000000000000000000, 1.000000000000000000, 1.000000000000000000, 1.000000000000000000, 1.000000000000000000, 1.000000000000000000, 1.000000000000000000, 1.000000000000000000, 1.000000000000000000, 1.000000000000000000, 1.000000000000000000, 1.000000000000000000, 1.000000000000000000, 1.000000000000000000, 1.000000000000000000, 1.000000000000000000, 1.000000000000000000, 1.000000000000000000, 1.000000000000000000, 1.000000000000000000, 1.000000000000000000, 1.000000000000000000, 1.000000000000000000, 1.000000000000000000, 1.000000000000000000, 1.000000000000000000, 1.000000000000000000, 1.000000000000000000, 1.000000000000000000, 1.000000000000000000, 1.000000000000000000, 1.000000000000000000, 1.000000000000000000, 1.000000000000000000, 1.000000000000000000, 1.000000000000000000, 1.000000000000000000, 1.000000000000000000, 1.000000000000000000, 1.000000000000000000, 1.000000000000000000, 1.000000000000000000, 1.000000000000000000, 1.000000000000000000, 1.000000000000000000, 1.000000000000000000, 1.000000000000000000, 1.000000000000000000, 1.000000000000000000, 1.000000000000000000, 1.000000000000000000, 1.000000000000000000, 1.000000000000000000, 1.000000000000000000, 1.000000000000000000, 1.000000000000000000, 1.000000000000000000, 1.000000000000000000, 1.000000000000000000, 1.000000000000000000, 1.000000000000000000, 1.000000000000000000, 1.000000000000000000, 1.000000000000000000, 1.000000000000000000, 1.000000000000000000, 1.000000000000000000, 1.000000000000000000, 1.000000000000000000, 1.000000000000000000, 1.000000000000000000, 1.000000000000000000, 1.000000000000000000, 1.000000000000000000, 1.000000000000000000, 1.000000000000000000, 1.000000000000000000, 1.000000000000000000, 1.000000000000000000, 1.000000000000000000, 1.000000000000000000, 1.000000000000000000, 1.000000000000000000, 1.000000000000000000, 1.000000000000000000, 1.000000000000000000, 1.000000000000000000, 1.000000000000000000, 1.000000000000000000, 1.000000000000000000, 1.000000000000000000, 1.000000000000000000, 1.000000000000000000, 1.000000000000000000, 1.000000000000000000, 1.000000000000000000, 1.000000000000000000, 1.000000000000000000, 1.000000000000000000, 1.000000000000000000, 1.000000000000000000, 1.000000000000000000, 1.000000000000000000, 1.000000000000000000, 1.000000000000000000, 1.000000000000000000, 1.000000000000000000, 1.000000000000000000, 1.000000000000000000, 1.000000000000000000, 1.000000000000000000, 1.000000000000000000, 1.000000000000000000, 1.000000000000000000, 1.000000000000000000, 1.000000000000000000, 1.000000000000000000, 1.000000000000000000, 1.000000000000000000, 1.000000000000000000),
 ( 0.3333333333333329818, 0.3333333333333329818, 0.3333333333333329818, 0.3333333333333329818, 0.3333333333333329818, 0.3333333333333329818, 0.3333333333333329818, 0.3333333333333329818, 0.3333333333333329818, 0.3333333333333329818, 0.3333333333333329818, 0.3333333333333329818, 0.3333333333333329818, 0.3333333333333329818, 0.3333333333333329818, 0.3333333333333329818, 0.3333333333333329818, 0.3333333333333329818, 0.3333333333333329818, 0.3333333333333329818, 0.3333333333333329818, 0.3333333333333329818, 0.3333333333333329818, 0.3333333333333329818, 0.3333333333333329818, 0.3333333333333329818, 0.3333333333333329818, 0.3333333333333329818, 0.3333333333333329818, 0.3333333333333329818, 0.3333333333333329818, 0.3333333333333329818, 0.3333333333333329818, 0.3333333333333329818, 0.3333333333333329818, 0.3333333333333329818, 0.3333333333333329818, 0.3333333333333329818, 0.3333333333333329818, 0.3333333333333329818, 0.3333333333333329818, 0.3333333333333329818, 0.3333333333333329818, 0.3333333333333329818, 0.3333333333333329818, 0.3333333333333329818, 0.3333333333333329818, 0.3333333333333329818, 0.3333333333333329818, 0.3333333333333329818, 0.3333333333333329818, 0.3333333333333329818, 0.3333333333333329818, 0.3333333333333329818, 0.3333333333333329818, 0.3333333333333329818, 0.3333333333333329818, 0.3333333333333329818, 0.3333333333333329818, 0.3333333333333329818, 0.3333333333333329818, 0.3333333333333329818, 0.3333333333333329818, 0.3333333333333329818, 0.3333333333333329818, 0.3333333333333329818, 0.3333333333333329818, 0.3333333333333329818, 0.3333333333333329818, 0.3333333333333329818, 0.3333333333333329818, 0.3333333333333329818, 0.3333333333333329818, 0.3333333333333329818, 0.3333333333333329818, 0.3333333333333329818, 0.3333333333333329818, 0.3333333333333329818, 0.3333333333333329818, 0.3333333333333329818, 0.3333333333333329818, 0.3333333333333329818, 0.3333333333333329818, 0.3333333333333329818, 0.3333333333333329818, 0.3333333333333329818, 0.3333333333333329818, 0.3333333333333329818, 0.3333333333333329818, 0.3333333333333329818, 0.3333333333333329818, 0.3333333333333329818, 0.3333333333333329818, 0.3333333333333329818, 0.3333333333333329818, 0.3333333333333329818, 0.3333333333333329818, 0.3333333333333329818, 0.3333333333333329818, 0.3333333333333329818, 0.3333333333333329818, 0.3333333333333329818, 0.3333333333333329818, 0.3333333333333329818, 0.3333333333333329818, 0.3333333333333329818, 0.3333333333333329818, 0.3333333333333329818, 0.3333333333333329818, 0.3333333333333329818, 0.3333333333333329818, 0.3333333333333329818, 0.3333333333333329818, 0.3333333333333329818, 0.3333333333333329818, 0.3333333333333329818, 0.3333333333333329818, 0.3333333333333329818, 0.3333333333333329818, 0.3333333333333329818, 0.3333333333333329818, 0.3333333333333329818, 0.3333333333333329818, 0.3333333333333329818, 0.3333333333333329818, 0.3333333333333329818, 0.3333333333333329818, 0.3333333333333329818, 0.3333333333333329818, 0.3333333333333329818, 0.3333333333333329818, 0.3333333333333329818, 0.3333333333333329818, 0.3333333333333329818, 0.3333333333333329818, 0.3333333333333329818, 0.3333333333333329818, 0.3333333333333329818, 0.3333333333333329818, 0.3333333333333329818, 0.3333333333333329818, 0.3333333333333329818, 0.3333333333333329818, 0.3333333333333329818, 0.3333333333333329818, 0.3333333333333329818, 0.3333333333333329818, 0.3333333333333329818, 0.3333333333333329818, 0.3333333333333329818, 0.3333333333333329818, 0.3333333333333329818, 0.3333333333333329818, 0.3333333333333329818, 0.3333333333333329818, 0.3333333333333329818, 0.3333333333333329818, 0.3333333333333329818, 0.3333333333333329818, 0.3333333333333329818, 0.3333333333333329818, 0.3333333333333329818, 0.3333333333333329818, 0.3333333333333329818, 0.3333333333333329818, 0.3333333333333329818, 0.3333333333333329818, 0.3333333333333329818, 0.3333333333333329818, 0.3333333333333329818, 0.3333333333333329818, 0.3333333333333329818, 0.3333333333333329818, 0.3333333333333329818, 0.3333333333333329818, 0.3333333333333329818, 0.3333333333333329818, 0.3333333333333329818, 0.3333333333333329818, 0.3333333333333329818, 0.3333333333333329818, 0.3333333333333329818, 0.3333333333333329818, 0.3333333333333329818, 0.3333333333333329818, 0.3333333333333329818, 0.3333333333333329818, 0.3333333333333329818),
 ( 0.3333333333333329818, 0.3333333333333329818, 0.3333333333333329818, 0.3333333333333329818, 0.3333333333333329818, 0.3333333333333329818, 0.3333333333333329818, 0.3333333333333329818, 0.3333333333333329818, 0.3333333333333329818, 0.3333333333333329818, 0.3333333333333329818, 0.3333333333333329818, 0.3333333333333329818, 0.3333333333333329818, 0.3333333333333329818, 0.3333333333333329818, 0.3333333333333329818, 0.3333333333333329818, 0.3333333333333329818, 0.3333333333333329818, 0.3333333333333329818, 0.3333333333333329818, 0.3333333333333329818, 0.3333333333333329818, 0.3333333333333329818, 0.3333333333333329818, 0.3333333333333329818, 0.3333333333333329818, 0.3333333333333329818, 0.3333333333333329818, 0.3333333333333329818, 0.3333333333333329818, 0.3333333333333329818, 0.3333333333333329818, 0.3333333333333329818, 0.3333333333333329818, 0.3333333333333329818, 0.3333333333333329818, 0.3333333333333329818, 0.3333333333333329818, 0.3333333333333329818, 0.3333333333333329818, 0.3333333333333329818, 0.3333333333333329818, 0.3333333333333329818, 0.3333333333333329818, 0.3333333333333329818, 0.3333333333333329818, 0.3333333333333329818, 0.3333333333333329818, 0.3333333333333329818, 0.3333333333333329818, 0.3333333333333329818, 0.3333333333333329818, 0.3333333333333329818, 0.3333333333333329818, 0.3333333333333329818, 0.3333333333333329818, 0.3333333333333329818, 0.3333333333333329818, 0.3333333333333329818, 0.3333333333333329818, 0.3333333333333329818, 0.3333333333333329818, 0.3333333333333329818, 0.3333333333333329818, 0.3333333333333329818, 0.3333333333333329818, 0.3333333333333329818, 0.3333333333333329818, 0.3333333333333329818, 0.3333333333333329818, 0.3333333333333329818, 0.3333333333333329818, 0.3333333333333329818, 0.3333333333333329818, 0.3333333333333329818, 0.3333333333333329818, 0.3333333333333329818, 0.3333333333333329818, 0.3333333333333329818, 0.3333333333333329818, 0.3333333333333329818, 0.3333333333333329818, 0.3333333333333329818, 0.3333333333333329818, 0.3333333333333329818, 0.3333333333333329818, 0.3333333333333329818, 0.3333333333333329818, 0.3333333333333329818, 0.3333333333333329818, 0.3333333333333329818, 0.3333333333333329818, 0.3333333333333329818, 0.3333333333333329818, 0.3333333333333329818, 0.3333333333333329818, 0.3333333333333329818, 0.3333333333333329818, 0.3333333333333329818, 0.3333333333333329818, 0.3333333333333329818, 0.3333333333333329818, 0.3333333333333329818, 0.3333333333333329818, 0.3333333333333329818, 0.3333333333333329818, 0.3333333333333329818, 0.3333333333333329818, 0.3333333333333329818, 0.3333333333333329818, 0.3333333333333329818, 0.3333333333333329818, 0.3333333333333329818, 0.3333333333333329818, 0.3333333333333329818, 0.3333333333333329818, 0.3333333333333329818, 0.3333333333333329818, 0.3333333333333329818, 0.3333333333333329818, 0.3333333333333329818, 0.3333333333333329818, 0.3333333333333329818, 0.3333333333333329818, 0.3333333333333329818, 0.3333333333333329818, 0.3333333333333329818, 0.3333333333333329818, 0.3333333333333329818, 0.3333333333333329818, 0.3333333333333329818, 0.3333333333333329818, 0.3333333333333329818, 0.3333333333333329818, 0.3333333333333329818, 0.3333333333333329818, 0.3333333333333329818, 0.3333333333333329818, 0.3333333333333329818, 0.3333333333333329818, 0.3333333333333329818, 0.3333333333333329818, 0.3333333333333329818, 0.3333333333333329818, 0.3333333333333329818, 0.3333333333333329818, 0.3333333333333329818, 0.3333333333333329818, 0.3333333333333329818, 0.3333333333333329818, 0.3333333333333329818, 0.3333333333333329818, 0.3333333333333329818, 0.3333333333333329818, 0.3333333333333329818, 0.3333333333333329818, 0.3333333333333329818, 0.3333333333333329818, 0.3333333333333329818, 0.3333333333333329818, 0.3333333333333329818, 0.3333333333333329818, 0.3333333333333329818, 0.3333333333333329818, 0.3333333333333329818, 0.3333333333333329818, 0.3333333333333329818, 0.3333333333333329818, 0.3333333333333329818, 0.3333333333333329818, 0.3333333333333329818, 0.3333333333333329818, 0.3333333333333329818, 0.3333333333333329818, 0.3333333333333329818, 0.3333333333333329818, 0.3333333333333329818, 0.3333333333333329818, 0.3333333333333329818, 0.3333333333333329818, 0.3333333333333329818, 0.3333333333333329818, 0.3333333333333329818, 0.3333333333333329818, 0.3333333333333329818),
 ( 1.000000000000000000, 1.000000000000000000, 1.000000000000000000, 1.000000000000000000, 1.000000000000000000, 1.000000000000000000, 1.000000000000000000, 1.000000000000000000, 1.000000000000000000, 1.000000000000000000, 1.000000000000000000, 1.000000000000000000, 1.000000000000000000, 1.000000000000000000, 1.000000000000000000, 1.000000000000000000, 1.000000000000000000, 1.000000000000000000, 1.000000000000000000, 1.000000000000000000, 1.000000000000000000, 1.000000000000000000, 1.000000000000000000, 1.000000000000000000, 1.000000000000000000, 1.000000000000000000, 1.000000000000000000, 1.000000000000000000, 1.000000000000000000, 1.000000000000000000, 1.000000000000000000, 1.000000000000000000, 1.000000000000000000, 1.000000000000000000, 1.000000000000000000, 1.000000000000000000, 1.000000000000000000, 1.000000000000000000, 1.000000000000000000, 1.000000000000000000, 1.000000000000000000, 1.000000000000000000, 1.000000000000000000, 1.000000000000000000, 1.000000000000000000, 1.000000000000000000, 1.000000000000000000, 1.000000000000000000, 1.000000000000000000, 1.000000000000000000, 1.000000000000000000, 1.000000000000000000, 1.000000000000000000, 1.000000000000000000, 1.000000000000000000, 1.000000000000000000, 1.000000000000000000, 1.000000000000000000, 1.000000000000000000, 1.000000000000000000, 1.000000000000000000, 1.000000000000000000, 1.000000000000000000, 1.000000000000000000, 1.000000000000000000, 1.000000000000000000, 1.000000000000000000, 1.000000000000000000, 1.000000000000000000, 1.000000000000000000, 1.000000000000000000, 1.000000000000000000, 1.000000000000000000, 1.000000000000000000, 1.000000000000000000, 1.000000000000000000, 1.000000000000000000, 1.000000000000000000, 1.000000000000000000, 1.000000000000000000, 1.000000000000000000, 1.000000000000000000, 1.000000000000000000, 1.000000000000000000, 1.000000000000000000, 1.000000000000000000, 1.000000000000000000, 1.000000000000000000, 1.000000000000000000, 1.000000000000000000, 1.000000000000000000, 1.000000000000000000, 1.000000000000000000, 1.000000000000000000, 1.000000000000000000, 1.000000000000000000, 1.000000000000000000, 1.000000000000000000, 1.000000000000000000, 1.000000000000000000, 1.000000000000000000, 1.000000000000000000, 1.000000000000000000, 1.000000000000000000, 1.000000000000000000, 1.000000000000000000, 1.000000000000000000, 1.000000000000000000, 1.000000000000000000, 1.000000000000000000, 1.000000000000000000, 1.000000000000000000, 1.000000000000000000, 1.000000000000000000, 1.000000000000000000, 1.000000000000000000, 1.000000000000000000, 1.000000000000000000, 1.000000000000000000, 1.000000000000000000, 1.000000000000000000, 1.000000000000000000, 1.000000000000000000, 1.000000000000000000, 1.000000000000000000, 1.000000000000000000, 1.000000000000000000, 1.000000000000000000, 1.000000000000000000, 1.000000000000000000, 1.000000000000000000, 1.000000000000000000, 1.000000000000000000, 1.000000000000000000, 1.000000000000000000, 1.000000000000000000, 1.000000000000000000, 1.000000000000000000, 1.000000000000000000, 1.000000000000000000, 1.000000000000000000, 1.000000000000000000, 1.000000000000000000, 1.000000000000000000, 1.000000000000000000, 1.000000000000000000, 1.000000000000000000, 1.000000000000000000, 1.000000000000000000, 1.000000000000000000, 1.000000000000000000, 1.000000000000000000, 1.000000000000000000, 1.000000000000000000, 1.000000000000000000, 1.000000000000000000, 1.000000000000000000, 1.000000000000000000, 1.000000000000000000, 1.000000000000000000, 1.000000000000000000, 1.000000000000000000, 1.000000000000000000, 1.000000000000000000, 1.000000000000000000, 1.000000000000000000, 1.000000000000000000, 1.000000000000000000, 1.000000000000000000, 1.000000000000000000, 1.000000000000000000, 1.000000000000000000, 1.000000000000000000, 1.000000000000000000, 1.000000000000000000, 1.000000000000000000, 1.000000000000000000, 1.000000000000000000, 1.000000000000000000, 1.000000000000000000, 1.000000000000000000, 1.000000000000000000, 1.000000000000000000, 1.000000000000000000, 1.000000000000000000, 1.000000000000000000, 1.000000000000000000, 1.000000000000000000) ) ) 
 REPRESENTATION_ITEM ( '' )  SURFACE ( )  );
#16595 = ORIENTED_EDGE ( 'NONE', *, *, #17038, .F. ) ;
#16596 = CARTESIAN_POINT ( 'NONE',  ( 0.9499999999999999556, 2.299999999999999822, 7.700000000000000178 ) ) ;
#16597 = CARTESIAN_POINT ( 'NONE',  ( 0.4974685680287860290, -5.139830508474580562, 7.000224381598740386 ) ) ;
#16598 = CARTESIAN_POINT ( 'NONE',  ( 1.250000000000000000, 3.500000000000000000, 5.100000000000000533 ) ) ;
#16599 = VECTOR ( 'NONE', #2148, 1000.000000000000000 ) ;
#16600 = EDGE_LOOP ( 'NONE', ( #2675, #5629, #17571, #7863 ) ) ;
#16601 = CARTESIAN_POINT ( 'NONE',  ( -1.571912189623050127, -1.264893411152959946, 6.451524409078659872 ) ) ;
#16602 = EDGE_CURVE ( 'NONE', #9670, #8456, #4941, .T. ) ;
#16603 = CARTESIAN_POINT ( 'NONE',  ( 1.800000000000000044, 11.40000000000000036, 6.599999999999999645 ) ) ;
#16604 = EDGE_CURVE ( 'NONE', #15023, #4272, #6242, .T. ) ;
#16605 = CARTESIAN_POINT ( 'NONE',  ( -0.3752419433106839453, -1.424070552810999812, 7.023346545710370314 ) ) ;
#16606 = CARTESIAN_POINT ( 'NONE',  ( 2.116444151961470066, -0.05338983050847490031, 3.670839500609349937 ) ) ;
#16607 = ORIENTED_EDGE ( 'NONE', *, *, #16055, .T. ) ;
#16608 = CARTESIAN_POINT ( 'NONE',  ( 2.353194804772640314, -0.3756355932203400139, 4.731327187377229571 ) ) ;
#16609 = VERTEX_POINT ( 'NONE', #8022 ) ;
#16610 = ORIENTED_EDGE ( 'NONE', *, *, #10898, .T. ) ;
#16611 = CARTESIAN_POINT ( 'NONE',  ( 0.1749999999999999889, 7.799999999999999822, 0.4000000000000000222 ) ) ;
#16612 = CARTESIAN_POINT ( 'NONE',  ( 1.507201387236019263, -2.475884402143949004, 6.507509243627190187 ) ) ;
#16613 =( NAMED_UNIT ( * ) SI_UNIT ( $, .STERADIAN. ) SOLID_ANGLE_UNIT ( ) );
#16614 = CARTESIAN_POINT ( 'NONE',  ( -1.707817112497179934, -5.488771186440679628, 6.319218296629480314 ) ) ;
#16615 = CARTESIAN_POINT ( 'NONE',  ( -2.608006145151089861, -1.427911429170979352, 5.191342690854409803 ) ) ;
#16616 = ORIENTED_EDGE ( 'NONE', *, *, #14001, .T. ) ;
#16617 = ADVANCED_FACE ( 'NONE', ( #13662 ), #14957, .F. ) ;
#16618 = CARTESIAN_POINT ( 'NONE',  ( -1.229686204202100175, -5.164643153926309793, 2.674737924334550154 ) ) ;
#16619 = CARTESIAN_POINT ( 'NONE',  ( -2.331386066015260106, -4.641695212954759953, 4.378465089518190467 ) ) ;
#16620 = CARTESIAN_POINT ( 'NONE',  ( -2.199635523370571111, -5.057043525783965876, 3.215170965529011493 ) ) ;
#16621 = EDGE_CURVE ( 'NONE', #10145, #17781, #11901, .T. ) ;
#16622 = CARTESIAN_POINT ( 'NONE',  ( 0.5999999999999999778, -7.347880794884110368E-17, 7.700000000000000178 ) ) ;
#16623 = DIRECTION ( 'NONE',  ( -1.000000000000000000, 1.480297366166869931E-15, 7.401486830834370362E-16 ) ) ;
#16624 = DIRECTION ( 'NONE',  ( 1.000000000000000000, 0.000000000000000000, 2.865091676452019757E-16 ) ) ;
#16625 = ADVANCED_FACE ( 'NONE', ( #3453, #7729, #9495, #14862, #5038 ), #15152, .F. ) ;
#16626 = CARTESIAN_POINT ( 'NONE',  ( -0.6965028529798926726, -1.470647129387581575, 6.631265289497783044 ) ) ;
#16627 = CARTESIAN_POINT ( 'NONE',  ( 1.000000000000000000, -6.000000000000000000, 3.299999999999999822 ) ) ;
#16628 = ORIENTED_EDGE ( 'NONE', *, *, #14600, .F. ) ;
#16629 = CARTESIAN_POINT ( 'NONE',  ( 7.069631497386979886E-16, 5.131370849898479136, 6.100000000000000533 ) ) ;
#16630 = CARTESIAN_POINT ( 'NONE',  ( 1.224646799147349904E-15, -10.00000000000000000, -6.123233995736771213E-16 ) ) ;
#16631 = CARTESIAN_POINT ( 'NONE',  ( 1.526871680339569659, -0.3400423728813561364, 3.327650196883443101 ) ) ;
#16632 = CARTESIAN_POINT ( 'NONE',  ( -2.445954350973251312, -2.941650167909708458, 5.729767452368195180 ) ) ;
#16633 = DIRECTION ( 'NONE',  ( 3.097720492815730124E-16, 1.000000000000000000, 0.000000000000000000 ) ) ;
#16634 = CARTESIAN_POINT ( 'NONE',  ( -0.009452110982656879157, -5.299807955295460005, 2.350000000000000089 ) ) ;
#16635 = CARTESIAN_POINT ( 'NONE',  ( 1.580445181003960586, -5.341949152542365908, 3.389704561770334301 ) ) ;
#16636 = ORIENTED_EDGE ( 'NONE', *, *, #1673, .F. ) ;
#16637 = PLANE ( 'NONE',  #30 ) ;
#16638 = CARTESIAN_POINT ( 'NONE',  ( 2.143090896833110381, -5.395338983050850246, 5.672454929438339732 ) ) ;
#16639 = DIRECTION ( 'NONE',  ( -2.220446049250309876E-16, -1.480297366166879989E-16, 1.000000000000000000 ) ) ;
#16640 = ORIENTED_EDGE ( 'NONE', *, *, #11485, .T. ) ;
#16641 = CARTESIAN_POINT ( 'NONE',  ( 1.300961508564179914, -5.422033898305079092, 6.661123742937279602 ) ) ;
#16642 = CARTESIAN_POINT ( 'NONE',  ( 2.352190863465239978, -0.6826862039457530784, 4.622903765856330338 ) ) ;
#16643 = CARTESIAN_POINT ( 'NONE',  ( -0.2938780505772099483, -3.706322805063249959, 2.062434951628528523 ) ) ;
#16644 = EDGE_CURVE ( 'NONE', #2681, #16120, #687, .T. ) ;
#16645 = LINE ( 'NONE', #18283, #10274 ) ;
#16646 = CARTESIAN_POINT ( 'NONE',  ( 1.934380261529039080, -0.7758393570989061683, 5.387804366397126010 ) ) ;
#16647 = CARTESIAN_POINT ( 'NONE',  ( 1.399999999999999911, -9.500000000000000000, 3.299999999999999822 ) ) ;
#16648 = CARTESIAN_POINT ( 'NONE',  ( -2.500000000000000000, 2.000000000000000000, 0.5999999999999999778 ) ) ;
#16649 = ORIENTED_EDGE ( 'NONE', *, *, #11069, .F. ) ;
#16650 = CARTESIAN_POINT ( 'NONE',  ( 0.9000000000000000222, 2.050000000000000266, 1.600000000000000089 ) ) ;
#16651 = CARTESIAN_POINT ( 'NONE',  ( -2.286166334984490067, -0.5135593220338989795, 5.258525443163870605 ) ) ;
#16652 = CARTESIAN_POINT ( 'NONE',  ( 2.352760675243219968, -2.565196678937129882, 4.757121734156020132 ) ) ;
#16653 = CARTESIAN_POINT ( 'NONE',  ( -2.293398556041709835, -0.5358050847457630494, 4.171956209133480975 ) ) ;
#16654 = LINE ( 'NONE', #2113, #10647 ) ;
#16655 = ADVANCED_FACE ( 'NONE', ( #781 ), #6419, .F. ) ;
#16656 = CARTESIAN_POINT ( 'NONE',  ( -2.350000000000000089, -6.000000000000000000, 2.799999999999999822 ) ) ;
#16657 = CARTESIAN_POINT ( 'NONE',  ( -2.088297318559229065, -5.202118644067799558, 5.785136623276640577 ) ) ;
#16658 = DIRECTION ( 'NONE',  ( 1.850371707708589879E-16, 1.000000000000000000, 0.000000000000000000 ) ) ;
#16659 = CARTESIAN_POINT ( 'NONE',  ( -0.003440977838562779990, -0.5045365850187280010, 2.491636233962229774 ) ) ;
#16660 = VERTEX_POINT ( 'NONE', #4115 ) ;
#16661 = CARTESIAN_POINT ( 'NONE',  ( -1.460675875430050175, -4.684430913171359734, 6.545310725710059785 ) ) ;
#16662 = EDGE_CURVE ( 'NONE', #6139, #6673, #9070, .T. ) ;
#16663 = CARTESIAN_POINT ( 'NONE',  ( 1.722095088963199405, -0.7763906680874423927, 2.675734922583239861 ) ) ;
#16664 = DIRECTION ( 'NONE',  ( -1.000000000000000000, 0.000000000000000000, 1.257750167763089819E-32 ) ) ;
#16665 = LINE ( 'NONE', #5554, #6835 ) ;
#16666 = CARTESIAN_POINT ( 'NONE',  ( 0.1749999999999999889, 9.099999999999999645, 0.4000000000000000222 ) ) ;
#16667 = CARTESIAN_POINT ( 'NONE',  ( 0.6673090596498160165, -2.239160642901090181, 2.443133963569570355 ) ) ;
#16668 = VECTOR ( 'NONE', #5293, 1000.000000000000000 ) ;
#16669 = CARTESIAN_POINT ( 'NONE',  ( 2.500000000000000000, 1.148961478048669885E-16, -2.399999999999999911 ) ) ;
#16670 = CARTESIAN_POINT ( 'NONE',  ( -0.9588981328681495109, -3.613169651910099756, 2.884671871696449230 ) ) ;
#16671 = DIRECTION ( 'NONE',  ( -1.000000000000000000, 0.000000000000000000, 0.000000000000000000 ) ) ;
#16672 = LINE ( 'NONE', #6668, #10046 ) ;
#16673 = ORIENTED_EDGE ( 'NONE', *, *, #18057, .F. ) ;
#16674 = DIRECTION ( 'NONE',  ( 0.000000000000000000, -1.000000000000000000, 0.000000000000000000 ) ) ;
#16675 = ORIENTED_EDGE ( 'NONE', *, *, #4729, .F. ) ;
#16676 = EDGE_LOOP ( 'NONE', ( #7697, #15208, #12311, #8997 ) ) ;
#16677 = ORIENTED_EDGE ( 'NONE', *, *, #15713, .T. ) ;
#16678 = DIRECTION ( 'NONE',  ( 1.000000000000000000, 0.000000000000000000, 0.000000000000000000 ) ) ;
#16679 = CARTESIAN_POINT ( 'NONE',  ( 0.6187874668174475623, -5.135381355932194580, 6.657494107589526422 ) ) ;
#16680 = DIRECTION ( 'NONE',  ( -2.114651788903909713E-47, 1.000000000000000000, -1.110223024625159992E-16 ) ) ;
#16681 = DIRECTION ( 'NONE',  ( 0.000000000000000000, 0.000000000000000000, -1.000000000000000000 ) ) ;
#16682 = CARTESIAN_POINT ( 'NONE',  ( -1.750000000000000000, 0.5999999999999999778, 7.550000000000000711 ) ) ;
#16683 = CARTESIAN_POINT ( 'NONE',  ( -0.9345217207511814506, -5.211074464177369414, 2.212378604467589494 ) ) ;
#16684 = CARTESIAN_POINT ( 'NONE',  ( 0.1749999999999999889, 9.099999999999999645, 0.4000000000000000222 ) ) ;
#16685 = CARTESIAN_POINT ( 'NONE',  ( -1.886482464143629967, -5.010466949207390108, 3.890008792968694618 ) ) ;
#16686 = CARTESIAN_POINT ( 'NONE',  ( 0.8570167067220200163, -0.01779661016949179997, 2.508190348879349774 ) ) ;
#16687 = VERTEX_POINT ( 'NONE', #4204 ) ;
#16688 = CARTESIAN_POINT ( 'NONE',  ( -2.500000000000000000, 10.00000000000000000, 1.600000000000000089 ) ) ;
#16689 = VECTOR ( 'NONE', #18020, 1000.000000000000000 ) ;
#16690 = VERTEX_POINT ( 'NONE', #18260 ) ;
#16691 = CARTESIAN_POINT ( 'NONE',  ( 2.230812463554230352, -0.1023305084745770588, 6.137473736419911674 ) ) ;
#16692 = CARTESIAN_POINT ( 'NONE',  ( 2.500000000000000000, 7.299999999999999822, 1.600000000000000089 ) ) ;
#16693 = VERTEX_POINT ( 'NONE', #16627 ) ;
#16694 = DIRECTION ( 'NONE',  ( 1.000000000000000000, 0.000000000000000000, 0.000000000000000000 ) ) ;
#16695 = CARTESIAN_POINT ( 'NONE',  ( 1.781655196750449255, -2.079983501243050092, 3.162323035427780482 ) ) ;
#16696 = CARTESIAN_POINT ( 'NONE',  ( -1.750316316486840051, -5.559957627118639500, 3.126818518378589928 ) ) ;
#16697 = CARTESIAN_POINT ( 'NONE',  ( -0.2041457401073759059, -1.101875393134940984, 7.346023093209487875 ) ) ;
#16698 = ORIENTED_EDGE ( 'NONE', *, *, #9850, .T. ) ;
#16699 = CARTESIAN_POINT ( 'NONE',  ( 0.5500000000000000444, 6.450000000000000178, 3.600000000000000089 ) ) ;
#16700 = CARTESIAN_POINT ( 'NONE',  ( -1.794646911016549939, -4.432100618360159672, 6.222494056560700315 ) ) ;
#16701 = DIRECTION ( 'NONE',  ( 1.823160359065819982E-16, 0.000000000000000000, -1.000000000000000000 ) ) ;
#16702 = CARTESIAN_POINT ( 'NONE',  ( -0.6628679656440369383, 6.450000000000000178, 1.670710678118660031 ) ) ;
#16703 = FACE_OUTER_BOUND ( 'NONE', #17722, .T. ) ;
#16704 = CARTESIAN_POINT ( 'NONE',  ( -1.823404397755031159, -1.656953435693890864, 5.643450181448764980 ) ) ;
#16705 = DIRECTION ( 'NONE',  ( 8.269460797427580527E-16, 8.934339325041029556E-19, -1.000000000000000000 ) ) ;
#16706 = LINE ( 'NONE', #12741, #1994 ) ;
#16707 = EDGE_CURVE ( 'NONE', #616, #747, #3928, .T. ) ;
#16708 = CARTESIAN_POINT ( 'NONE',  ( -1.668426559427188982, -4.385524041783587457, 6.763847501343006385 ) ) ;
#16709 = DIRECTION ( 'NONE',  ( 0.000000000000000000, 2.220446049250309876E-16, -1.000000000000000000 ) ) ;
#16710 = CARTESIAN_POINT ( 'NONE',  ( -0.3865907654992132292, -4.952022267818764867, 2.675656795012148592 ) ) ;
#16711 = CARTESIAN_POINT ( 'NONE',  ( -2.052786957354850728, -5.224364406779660186, 4.727327971967373976 ) ) ;
#16712 = ORIENTED_EDGE ( 'NONE', *, *, #5201, .T. ) ;
#16713 = EDGE_CURVE ( 'NONE', #10138, #13931, #15340, .T. ) ;
#16714 = CARTESIAN_POINT ( 'NONE',  ( 2.270487904532159540, -0.06228813559322070315, 4.080813552109670894 ) ) ;
#16715 = EDGE_CURVE ( 'NONE', #12725, #6904, #9950, .T. ) ;
#16716 = LINE ( 'NONE', #11164, #4385 ) ;
#16717 = CARTESIAN_POINT ( 'NONE',  ( 0.5500000000000000444, 6.450000000000000178, 3.200000000000000178 ) ) ;
#16718 = EDGE_CURVE ( 'NONE', #16897, #3896, #6810, .T. ) ;
#16719 = ORIENTED_EDGE ( 'NONE', *, *, #17100, .T. ) ;
#16720 = CARTESIAN_POINT ( 'NONE',  ( -1.889104232906369862, -5.555508474576269506, 3.296507079072529933 ) ) ;
#16721 = CARTESIAN_POINT ( 'NONE',  ( -1.864786684738369837, -4.804713230972779137, 2.817120744449669978 ) ) ;
#16722 = CARTESIAN_POINT ( 'NONE',  ( 1.899999999999999911, 9.199999999999999289, 0.6099999999999999867 ) ) ;
#16723 = CARTESIAN_POINT ( 'NONE',  ( -1.632144308286139989, -1.311469987729540376, 5.945394234592896510 ) ) ;
#16724 = VECTOR ( 'NONE', #13657, 1000.000000000000000 ) ;
#16725 = LINE ( 'NONE', #9603, #16765 ) ;
#16726 = ORIENTED_EDGE ( 'NONE', *, *, #10377, .F. ) ;
#16727 = CARTESIAN_POINT ( 'NONE',  ( 1.768982498583140162, -5.182556448558739426, 2.931017501416850024 ) ) ;
#16728 = CARTESIAN_POINT ( 'NONE',  ( -0.9150601050661559821, -0.4690677966101700069, 6.868218666554230190 ) ) ;
#16729 = CARTESIAN_POINT ( 'NONE',  ( -1.917298190932639868, -3.496728210468659892, 3.335187436117939885 ) ) ;
#16730 = LINE ( 'NONE', #16830, #8956 ) ;
#16731 = CARTESIAN_POINT ( 'NONE',  ( -1.899999999999999911, 10.00000000000000000, 1.600000000000000089 ) ) ;
#16732 = CARTESIAN_POINT ( 'NONE',  ( -2.638803263991410741, -5.519915254237295343, 4.982085668537435730 ) ) ;
#16733 = VERTEX_POINT ( 'NONE', #6710 ) ;
#16734 = PRODUCT_DEFINITION_SHAPE ( 'NONE', 'NONE',  #18299 ) ;
#16735 = EDGE_CURVE ( 'NONE', #2376, #17417, #9581, .T. ) ;
#16736 = CIRCLE ( 'NONE', #13485, 0.01000000000000002623 ) ;
#16737 = ORIENTED_EDGE ( 'NONE', *, *, #15047, .F. ) ;
#16738 = FACE_OUTER_BOUND ( 'NONE', #11783, .T. ) ;
#16739 = FACE_OUTER_BOUND ( 'NONE', #8256, .T. ) ;
#16740 = CARTESIAN_POINT ( 'NONE',  ( -0.009452173233711079481, -0.5998089419219779783, 2.358866582356790254 ) ) ;
#16741 = CIRCLE ( 'NONE', #8755, 0.2500000000000002220 ) ;
#16742 = ORIENTED_EDGE ( 'NONE', *, *, #9822, .T. ) ;
#16743 = CIRCLE ( 'NONE', #11123, 0.6324555320336745501 ) ;
#16744 = AXIS2_PLACEMENT_3D ( 'NONE', #2505, #13330, #9450 ) ;
#16745 = CARTESIAN_POINT ( 'NONE',  ( 0.4005155088302400634, -4.474836318576759453, 7.019123328904770531 ) ) ;
#16746 = CARTESIAN_POINT ( 'NONE',  ( 0.4944444514933294954, -5.311531839079339790, 2.693008931300498787 ) ) ;
#16747 = LINE ( 'NONE', #6935, #11595 ) ;
#16748 = CARTESIAN_POINT ( 'NONE',  ( -0.6628679656440369383, 6.450000000000000178, 1.670710678118660031 ) ) ;
#16749 = CARTESIAN_POINT ( 'NONE',  ( -1.097561405233230092, -3.613169651910099756, 2.618148744692269769 ) ) ;
#16750 = DIRECTION ( 'NONE',  ( -1.224646799147351975E-16, 1.000000000000000000, 6.123233995736759873E-17 ) ) ;
#16751 = CARTESIAN_POINT ( 'NONE',  ( 1.472933559740161602, -2.751502985243430288, 6.130163826706326091 ) ) ;
#16752 = VECTOR ( 'NONE', #15517, 1000.000000000000000 ) ;
#16753 = DIRECTION ( 'NONE',  ( 0.000000000000000000, -3.152456273542039042E-16, -1.000000000000000000 ) ) ;
#16754 = CARTESIAN_POINT ( 'NONE',  ( -0.1641805561540918557, -0.5962015548080631389, 2.650681144176719961 ) ) ;
#16755 = VERTEX_POINT ( 'NONE', #5607 ) ;
#16756 = EDGE_CURVE ( 'NONE', #17179, #2455, #7604, .T. ) ;
#16757 = CYLINDRICAL_SURFACE ( 'NONE', #14302, 0.1000000000000000472 ) ;
#16758 = CARTESIAN_POINT ( 'NONE',  ( -2.218077401483159683, -4.824160642901089702, 5.486688202856539576 ) ) ;
#16759 = VERTEX_POINT ( 'NONE', #11252 ) ;
#16760 = AXIS2_PLACEMENT_3D ( 'NONE', #14310, #12750, #4215 ) ;
#16761 = VERTEX_POINT ( 'NONE', #18156 ) ;
#16762 = LINE ( 'NONE', #9738, #6443 ) ;
#16763 = CARTESIAN_POINT ( 'NONE',  ( -1.647941990407690627, -5.255508474576275901, 3.475676388127094896 ) ) ;
#16764 = CARTESIAN_POINT ( 'NONE',  ( 1.650842931266089497, -2.033406924666469884, 2.622060802311419803 ) ) ;
#16765 = VECTOR ( 'NONE', #12477, 1000.000000000000000 ) ;
#16766 = LINE ( 'NONE', #1401, #5257 ) ;
#16767 =( GEOMETRIC_REPRESENTATION_CONTEXT ( 3 ) GLOBAL_UNCERTAINTY_ASSIGNED_CONTEXT ( ( #2701 ) ) GLOBAL_UNIT_ASSIGNED_CONTEXT ( ( #6020, #16109, #381 ) ) REPRESENTATION_CONTEXT ( 'NONE', 'WORKASPACE' ) );
#16768 = LINE ( 'NONE', #12603, #8785 ) ;
#16769 = DIRECTION ( 'NONE',  ( 0.000000000000000000, 0.000000000000000000, -1.000000000000000000 ) ) ;
#16770 = AXIS2_PLACEMENT_3D ( 'NONE', #1075, #6719, #18269 ) ;
#16771 = DIRECTION ( 'NONE',  ( -1.000000000000000000, 0.000000000000000000, 0.000000000000000000 ) ) ;
#16772 = LINE ( 'NONE', #1407, #9384 ) ;
#16773 = CARTESIAN_POINT ( 'NONE',  ( 2.046174187462399985, -1.121322805063259986, 5.862719605943959245 ) ) ;
#16774 = AXIS2_PLACEMENT_3D ( 'NONE', #16506, #5206, #3820 ) ;
#16775 = STYLED_ITEM ( 'NONE', ( #380 ), #7785 ) ;
#16776 = CARTESIAN_POINT ( 'NONE',  ( 1.454969160282001406, -2.452596113855660676, 6.148435909958180901 ) ) ;
#16777 = VECTOR ( 'NONE', #5873, 1000.000000000000000 ) ;
#16778 = CARTESIAN_POINT ( 'NONE',  ( 2.340070819011249803, -0.08008474576271229495, 4.950151441910540129 ) ) ;
#16779 = VERTEX_POINT ( 'NONE', #15522 ) ;
#16780 = EDGE_LOOP ( 'NONE', ( #181, #1498, #11818, #8868 ) ) ;
#16781 = ADVANCED_FACE ( 'NONE', ( #1067 ), #1164, .T. ) ;
#16782 = AXIS2_PLACEMENT_3D ( 'NONE', #2826, #15615, #5700 ) ;
#16783 = CARTESIAN_POINT ( 'NONE',  ( 2.088297318559229954, -0.09788135593220401165, 5.785136623276629919 ) ) ;
#16784 = AXIS2_PLACEMENT_3D ( 'NONE', #14230, #3200, #1550 ) ;
#16785 = CARTESIAN_POINT ( 'NONE',  ( 1.399999999999999911, -6.000000000000000000, 3.299999999999999822 ) ) ;
#16786 = ORIENTED_EDGE ( 'NONE', *, *, #9492, .F. ) ;
#16787 = CARTESIAN_POINT ( 'NONE',  ( -0.6914213562373099364, 6.450000000000000178, 2.557842712474620139 ) ) ;
#16788 = ORIENTED_EDGE ( 'NONE', *, *, #216, .T. ) ;
#16789 = CARTESIAN_POINT ( 'NONE',  ( -2.245209214543379961, -2.964938456198000782, 5.405536158119060630 ) ) ;
#16790 = CARTESIAN_POINT ( 'NONE',  ( 2.321479326063749404, -5.350847457627126325, 3.414080590619961608 ) ) ;
#16791 = VECTOR ( 'NONE', #7039, 1000.000000000000000 ) ;
#16792 = CIRCLE ( 'NONE', #8220, 0.1999999999999998168 ) ;
#16793 = ORIENTED_EDGE ( 'NONE', *, *, #11569, .F. ) ;
#16794 = CARTESIAN_POINT ( 'NONE',  ( 1.936998685628529948, -0.8418633456037969420, 3.363294429306519895 ) ) ;
#16795 = CARTESIAN_POINT ( 'NONE',  ( -1.880631435828179265, -0.5447033898305090327, 3.876649216148230437 ) ) ;
#16796 = VERTEX_POINT ( 'NONE', #8473 ) ;
#16797 = CIRCLE ( 'NONE', #8224, 0.2000000000000000389 ) ;
#16798 = DIRECTION ( 'NONE',  ( -1.000000000000000000, 6.098637220230962441E-16, 0.000000000000000000 ) ) ;
#16799 = AXIS2_PLACEMENT_3D ( 'NONE', #10181, #6206, #5935 ) ;
#16800 = CARTESIAN_POINT ( 'NONE',  ( -1.440522616026439495, -4.804713230972779137, 3.241384813161591438 ) ) ;
#16801 = FACE_OUTER_BOUND ( 'NONE', #17699, .T. ) ;
#16802 = DIRECTION ( 'NONE',  ( 3.700743415417190309E-15, -6.579099405186109509E-16, 1.000000000000000000 ) ) ;
#16803 = AXIS2_PLACEMENT_3D ( 'NONE', #74, #16998, #4314 ) ;
#16804 = PLANE ( 'NONE',  #7044 ) ;
#16805 = VECTOR ( 'NONE', #5928, 1000.000000000000000 ) ;
#16806 = CARTESIAN_POINT ( 'NONE',  ( -1.949083719010310078, -0.2402542372881359412, 4.055210292801460170 ) ) ;
#16807 = CARTESIAN_POINT ( 'NONE',  ( 2.612083973477990373, -3.780028546288090041, 4.230818789270793800 ) ) ;
#16808 = CARTESIAN_POINT ( 'NONE',  ( -0.009452110982656879157, -5.299807955295460005, 2.350000000000000089 ) ) ;
#16809 = CARTESIAN_POINT ( 'NONE',  ( 1.449568901432419343, -5.337500000000000355, 3.250431098567584165 ) ) ;
#16810 = ORIENTED_EDGE ( 'NONE', *, *, #17253, .T. ) ;
#16811 = CIRCLE ( 'NONE', #1736, 0.9499999999999999556 ) ;
#16812 = CARTESIAN_POINT ( 'NONE',  ( 1.428515267734869587, -0.03114406779661050076, 2.829745655876920285 ) ) ;
#16813 = CARTESIAN_POINT ( 'NONE',  ( 1.850000000000000089, -5.599999999999999645, 2.799999999999999822 ) ) ;
#16814 = CARTESIAN_POINT ( 'NONE',  ( -1.873832970144350130, -0.5625000000000005551, 2.826167029855650270 ) ) ;
#16815 = ORIENTED_EDGE ( 'NONE', *, *, #13452, .T. ) ;
#16816 = LINE ( 'NONE', #4130, #7895 ) ;
#16817 = VECTOR ( 'NONE', #11856, 1000.000000000000000 ) ;
#16818 = VECTOR ( 'NONE', #7330, 1000.000000000000000 ) ;
#16819 = CARTESIAN_POINT ( 'NONE',  ( -0.5606293434988356417, -4.269082600342137823, 7.293994686233948421 ) ) ;
#16820 = FACE_OUTER_BOUND ( 'NONE', #17113, .T. ) ;
#16821 = CARTESIAN_POINT ( 'NONE',  ( 1.117157304995380240, -0.9388573751169233539, 6.422457952614097465 ) ) ;
#16822 = ADVANCED_FACE ( 'NONE', ( #16801 ), #14110, .T. ) ;
#16823 = DIRECTION ( 'NONE',  ( -1.000000000000000000, 0.000000000000000000, 0.000000000000000000 ) ) ;
#16824 = VERTEX_POINT ( 'NONE', #12367 ) ;
#16825 = EDGE_CURVE ( 'NONE', #84, #6428, #8298, .T. ) ;
#16826 = CARTESIAN_POINT ( 'NONE',  ( -1.661700935788390066, -4.954166666666670160, 3.038299064211620326 ) ) ;
#16827 = CARTESIAN_POINT ( 'NONE',  ( -1.641808337277740115, -0.4868644067796619734, 6.386111670537629514 ) ) ;
#16828 = AXIS2_PLACEMENT_3D ( 'NONE', #2294, #12200, #17816 ) ;
#16829 = CARTESIAN_POINT ( 'NONE',  ( -1.781655196750479897, -3.520016498756949996, 3.162323035427820450 ) ) ;
#16830 = CARTESIAN_POINT ( 'NONE',  ( -1.550000000000000044, -5.599999999999999645, 5.100000000000000533 ) ) ;
#16831 = CARTESIAN_POINT ( 'NONE',  ( 1.000000000000000000, -8.000000000000000000, 5.700000000000000178 ) ) ;
#16832 = CARTESIAN_POINT ( 'NONE',  ( -1.610878918935079840, -5.568855932203385706, 2.590989782159090815 ) ) ;
#16833 = ORIENTED_EDGE ( 'NONE', *, *, #9390, .F. ) ;
#16834 = EDGE_LOOP ( 'NONE', ( #16261, #14184, #5297, #8451 ) ) ;
#16835 = DIRECTION ( 'NONE',  ( 0.000000000000000000, -1.000000000000000000, 6.530723674265619530E-17 ) ) ;
#16836 = DIRECTION ( 'NONE',  ( 0.000000000000000000, 0.000000000000000000, 1.000000000000000000 ) ) ;
#16837 = FACE_OUTER_BOUND ( 'NONE', #16155, .T. ) ;
#16838 = ORIENTED_EDGE ( 'NONE', *, *, #2719, .F. ) ;
#16839 = CARTESIAN_POINT ( 'NONE',  ( -0.2564439965878500538, -4.544701183441629766, 7.039440566481220074 ) ) ;
#16840 = EDGE_CURVE ( 'NONE', #6456, #11596, #15241, .T. ) ;
#16841 = DIRECTION ( 'NONE',  ( -2.612289469706250277E-16, 1.000000000000000000, 0.000000000000000000 ) ) ;
#16842 = CARTESIAN_POINT ( 'NONE',  ( 0.9788656693287738353, -5.320452325212859712, 2.556357798777459944 ) ) ;
#16843 = VECTOR ( 'NONE', #11949, 1000.000000000000000 ) ;
#16844 = LINE ( 'NONE', #18032, #4489 ) ;
#16845 = EDGE_CURVE ( 'NONE', #9321, #17934, #5422, .T. ) ;
#16846 = PLANE ( 'NONE',  #3737 ) ;
#16847 = CARTESIAN_POINT ( 'NONE',  ( -1.914021115237000137, -4.754295778036220277, 6.069404563272239983 ) ) ;
#16848 = ADVANCED_FACE ( 'NONE', ( #8194 ), #14021, .T. ) ;
#16849 = CARTESIAN_POINT ( 'NONE',  ( 1.800000000000000044, 0.5999999999999999778, 7.550000000000000711 ) ) ;
#16850 = EDGE_CURVE ( 'NONE', #7434, #4810, #15435, .T. ) ;
#16851 = CARTESIAN_POINT ( 'NONE',  ( -1.865240315818168959, -3.450151633892079239, 3.842223568244830467 ) ) ;
#16852 = FACE_BOUND ( 'NONE', #10338, .T. ) ;
#16853 = B_SPLINE_CURVE_WITH_KNOTS ( 'NONE', 3,
 ( #705, #6257, #14680, #4960, #1998, #7744, #13300 ),
 .UNSPECIFIED., .F., .F.,
 ( 4, 1, 1, 1, 4 ),
 ( 0.000000000000000000, 0.3003308066897660278, 0.4325493167368040237, 0.5576349185195599301, 0.7853981633974479459 ),
 .UNSPECIFIED. ) ;
#16854 = VERTEX_POINT ( 'NONE', #16979 ) ;
#16855 = LINE ( 'NONE', #12788, #9765 ) ;
#16856 = VERTEX_POINT ( 'NONE', #8569 ) ;
#16857 = LINE ( 'NONE', #9823, #3956 ) ;
#16858 = ORIENTED_EDGE ( 'NONE', *, *, #5093, .F. ) ;
#16859 = VECTOR ( 'NONE', #8595, 1000.000000000000000 ) ;
#16860 = VERTEX_POINT ( 'NONE', #7266 ) ;
#16861 = ORIENTED_EDGE ( 'NONE', *, *, #7598, .T. ) ;
#16862 = DIRECTION ( 'NONE',  ( 2.018587317500279868E-16, -1.000000000000000000, -5.046468293750709530E-17 ) ) ;
#16863 = CARTESIAN_POINT ( 'NONE',  ( -0.9222751404131093178, -5.277754237288146300, 2.865854510788139908 ) ) ;
#16864 = CARTESIAN_POINT ( 'NONE',  ( 0.2938780505771511620, -1.893677194936738806, 2.062434951628520086 ) ) ;
#16865 = DIRECTION ( 'NONE',  ( 0.000000000000000000, 1.000000000000000000, 0.000000000000000000 ) ) ;
#16866 = LINE ( 'NONE', #14272, #1101 ) ;
#16867 = LINE ( 'NONE', #8272, #169 ) ;
#16868 = EDGE_CURVE ( 'NONE', #8419, #9933, #14215, .T. ) ;
#16869 = DIRECTION ( 'NONE',  ( -1.048990684667790150E-15, 0.000000000000000000, -1.000000000000000000 ) ) ;
#16870 = VECTOR ( 'NONE', #5967, 1000.000000000000000 ) ;
#16871 = CARTESIAN_POINT ( 'NONE',  ( -0.4201920264140019956, -2.122719201459649874, 2.384360920086639801 ) ) ;
#16872 = CARTESIAN_POINT ( 'NONE',  ( -1.810994336139479133, -2.918361879621429011, 5.667058093962724641 ) ) ;
#16873 = CARTESIAN_POINT ( 'NONE',  ( 0.06367493584606445656, -0.001483050847457929866, 2.649999999999998579 ) ) ;
#16874 = ORIENTED_EDGE ( 'NONE', *, *, #148, .F. ) ;
#16875 = CARTESIAN_POINT ( 'NONE',  ( 2.011500846714319835, -0.3489406779661020086, 3.478373409938460448 ) ) ;
#16876 = CARTESIAN_POINT ( 'NONE',  ( 2.345900685764729765, -0.3711864406779670222, 4.512231114381330066 ) ) ;
#16877 = DIRECTION ( 'NONE',  ( 1.000000000000000000, 0.000000000000000000, 0.000000000000000000 ) ) ;
#16878 = ORIENTED_EDGE ( 'NONE', *, *, #5071, .F. ) ;
#16879 = CARTESIAN_POINT ( 'NONE',  ( -1.641808337277740115, -0.1868644067796620123, 6.386111670537629514 ) ) ;
#16880 = CARTESIAN_POINT ( 'NONE',  ( 0.7109160811436110450, -1.307629111369560171, 6.943511536198400336 ) ) ;
#16881 = ORIENTED_EDGE ( 'NONE', *, *, #15261, .T. ) ;
#16882 = EDGE_LOOP ( 'NONE', ( #9547, #3537, #2813, #3564 ) ) ;
#16883 = EDGE_CURVE ( 'NONE', #16255, #10849, #11602, .T. ) ;
#16884 = CARTESIAN_POINT ( 'NONE',  ( -0.7678268402137429227, -2.732055573315121055, 6.924676972266150088 ) ) ;
#16885 = VECTOR ( 'NONE', #13298, 1000.000000000000114 ) ;
#16886 = CARTESIAN_POINT ( 'NONE',  ( -0.1765068388402301069, -5.453177966101685037, 7.347961541693632803 ) ) ;
#16887 = ORIENTED_EDGE ( 'NONE', *, *, #11183, .F. ) ;
#16888 = CARTESIAN_POINT ( 'NONE',  ( 1.303621121494459967, -1.237764246504700072, 6.659417683669679455 ) ) ;
#16889 = CARTESIAN_POINT ( 'NONE',  ( 0.6964468257805941365, -0.4334745762711874617, 6.631228347243847132 ) ) ;
#16890 = ORIENTED_EDGE ( 'NONE', *, *, #7000, .F. ) ;
#16891 = EDGE_CURVE ( 'NONE', #4627, #16693, #3277, .T. ) ;
#16892 = CARTESIAN_POINT ( 'NONE',  ( -0.03000000000000159830, 11.40000000000000036, 7.649999999999999467 ) ) ;
#16893 = CARTESIAN_POINT ( 'NONE',  ( 1.149999999999999911, 9.248236190979499227, 7.693185165257809821 ) ) ;
#16894 = CARTESIAN_POINT ( 'NONE',  ( 1.899999999999999911, 0.5999999999999999778, 0.5999999999999999778 ) ) ;
#16895 = CARTESIAN_POINT ( 'NONE',  ( -2.033547680391670998, -4.641695212954759064, 4.417890669792460479 ) ) ;
#16896 = PRODUCT_DEFINITION_SHAPE ( 'NONE', 'NONE',  #18293 ) ;
#16897 = VERTEX_POINT ( 'NONE', #4741 ) ;
#16898 = DIRECTION ( 'NONE',  ( -1.000000000000000000, 0.000000000000000000, 0.000000000000000000 ) ) ;
#16899 = DIRECTION ( 'NONE',  ( 0.000000000000000000, 6.123233995736769734E-17, -1.000000000000000000 ) ) ;
#16900 = CARTESIAN_POINT ( 'NONE',  ( 2.022304719220918479, -0.3667372881355940861, 4.346496488058688712 ) ) ;
#16901 = CARTESIAN_POINT ( 'NONE',  ( 2.358786130710011086, -3.943046564306109669, 5.916240799583690979 ) ) ;
#16902 = DIRECTION ( 'NONE',  ( 1.000000000000000000, 0.000000000000000000, 0.000000000000000000 ) ) ;
#16903 = CARTESIAN_POINT ( 'NONE',  ( -2.022304719220918479, -5.233262711864406391, 4.346496488058700258 ) ) ;
#16904 = EDGE_LOOP ( 'NONE', ( #370, #8638, #15084 ) ) ;
#16905 = DIRECTION ( 'NONE',  ( -2.220446049250319983E-16, 0.000000000000000000, -1.000000000000000000 ) ) ;
#16906 = CARTESIAN_POINT ( 'NONE',  ( -0.6500000000000000222, 3.050000000000000266, 3.200000000000000178 ) ) ;
#16907 = DIRECTION ( 'NONE',  ( -1.000000000000000000, 2.960594732333750117E-16, 0.000000000000000000 ) ) ;
#16908 = EDGE_LOOP ( 'NONE', ( #5785, #12024, #6273, #5690 ) ) ;
#16909 = CARTESIAN_POINT ( 'NONE',  ( 0.5999999999999999778, 10.80000000000000071, 7.599999999999999645 ) ) ;
#16910 = CARTESIAN_POINT ( 'NONE',  ( -1.728413393879669968, -1.288181699441249828, 6.297289212178331042 ) ) ;
#16911 = DIRECTION ( 'NONE',  ( 0.000000000000000000, 0.000000000000000000, 1.000000000000000000 ) ) ;
#16912 = CARTESIAN_POINT ( 'NONE',  ( 1.668733558229380520, -0.8457042219637719294, 5.895922302771890777 ) ) ;
#16913 = APPLICATION_CONTEXT ( 'automotive_design' ) ;
#16914 = CARTESIAN_POINT ( 'NONE',  ( 0.1749999999999999889, 9.500000000000000000, 1.600000000000000089 ) ) ;
#16915 = ORIENTED_EDGE ( 'NONE', *, *, #4820, .T. ) ;
#16916 = DIRECTION ( 'NONE',  ( 1.060879779086260081E-14, -8.223874256482640091E-16, 1.000000000000000000 ) ) ;
#16917 = CARTESIAN_POINT ( 'NONE',  ( -0.06264882350515391107, -0.4512711864406790396, 7.052569299041220319 ) ) ;
#16918 = CARTESIAN_POINT ( 'NONE',  ( -0.4790341583531910197, -3.683034516774959855, 2.395814251711740006 ) ) ;
#16919 = CARTESIAN_POINT ( 'NONE',  ( -0.2749999999999995781, 2.299999999999999822, 7.599999999999999645 ) ) ;
#16920 = LINE ( 'NONE', #7554, #17432 ) ;
#16921 = ORIENTED_EDGE ( 'NONE', *, *, #8331, .T. ) ;
#16922 = VERTEX_POINT ( 'NONE', #10391 ) ;
#16923 = CARTESIAN_POINT ( 'NONE',  ( -0.6914213562373099364, 6.450000000000000178, 2.557842712474620139 ) ) ;
#16924 = CARTESIAN_POINT ( 'NONE',  ( 2.500000000000000000, 11.25000000000000000, 7.649999999999999467 ) ) ;
#16925 = PLANE ( 'NONE',  #10007 ) ;
#16926 = EDGE_LOOP ( 'NONE', ( #13778, #10477, #16649, #15967 ) ) ;
#16927 = EDGE_CURVE ( 'NONE', #2194, #917, #9986, .T. ) ;
#16928 = CARTESIAN_POINT ( 'NONE',  ( 2.579602008086750775, -1.051457940198389673, 5.323511966907245707 ) ) ;
#16929 = DIRECTION ( 'NONE',  ( 1.224646799147350002E-16, -1.000000000000000000, -6.123233995736769734E-17 ) ) ;
#16930 = CARTESIAN_POINT ( 'NONE',  ( -2.343457872958619959, -1.451199717459269900, 4.916681529328609912 ) ) ;
#16931 = DIRECTION ( 'NONE',  ( -6.162975822039159109E-32, -1.000000000000000000, -1.110223024625159992E-16 ) ) ;
#16932 = CARTESIAN_POINT ( 'NONE',  ( 2.311987889326980294, -4.078935417675859654, 4.260161748947079552 ) ) ;
#16933 = LINE ( 'NONE', #1922, #9334 ) ;
#16934 = CARTESIAN_POINT ( 'NONE',  ( -2.051695471449629160, -3.333710192450643373, 4.773807418740784847 ) ) ;
#16935 = CARTESIAN_POINT ( 'NONE',  ( 0.1749999999999999889, 7.500000000000000000, 1.600000000000000089 ) ) ;
#16936 = CARTESIAN_POINT ( 'NONE',  ( 0.5372984490435490645, 4.250000000000000000, 7.700000000000000178 ) ) ;
#16937 = ORIENTED_EDGE ( 'NONE', *, *, #13815, .F. ) ;
#16938 = CARTESIAN_POINT ( 'NONE',  ( -1.496290472746829803, -0.5672554343907050267, 2.872674968141029961 ) ) ;
#16939 = ORIENTED_EDGE ( 'NONE', *, *, #4482, .T. ) ;
#16940 = EDGE_CURVE ( 'NONE', #2455, #16733, #13002, .T. ) ;
#16941 = FACE_OUTER_BOUND ( 'NONE', #17950, .T. ) ;
#16942 = ORIENTED_EDGE ( 'NONE', *, *, #14700, .T. ) ;
#16943 = CARTESIAN_POINT ( 'NONE',  ( 1.000000000000000000, -5.500000000000000000, 5.100000000000000533 ) ) ;
#16944 = EDGE_CURVE ( 'NONE', #13978, #15121, #7361, .T. ) ;
#16945 = ORIENTED_EDGE ( 'NONE', *, *, #9255, .T. ) ;
#16946 = EDGE_CURVE ( 'NONE', #16796, #2415, #3296, .T. ) ;
#16947 = CARTESIAN_POINT ( 'NONE',  ( 2.000624272291700034, -5.064194915254235596, 4.239366054775996595 ) ) ;
#16948 = ADVANCED_FACE ( 'NONE', ( #1825 ), #11819, .F. ) ;
#16949 = CARTESIAN_POINT ( 'NONE',  ( -2.105672170043390246, -1.637506023765568530, 3.084680091961149007 ) ) ;
#16950 = CARTESIAN_POINT ( 'NONE',  ( -1.800000000000000044, 11.40000000000000036, 6.599999999999999645 ) ) ;
#16951 = DIRECTION ( 'NONE',  ( -0.7071067811865489050, 0.000000000000000000, 0.7071067811865461294 ) ) ;
#16952 = CARTESIAN_POINT ( 'NONE',  ( 1.875000000000000000, -2.296212748401290437E-16, 7.700000000000000178 ) ) ;
#16953 = AXIS2_PLACEMENT_3D ( 'NONE', #15806, #3112, #8764 ) ;
#16954 = DIRECTION ( 'NONE',  ( 1.000000000000000000, 0.000000000000000000, 0.000000000000000000 ) ) ;
#16955 = DIRECTION ( 'NONE',  ( 0.000000000000000000, -1.000000000000000000, 0.000000000000000000 ) ) ;
#16956 = CARTESIAN_POINT ( 'NONE',  ( -0.9485663501270049647, -3.054250732991179440, 6.853826262002260528 ) ) ;
#16957 = CARTESIAN_POINT ( 'NONE',  ( -1.893291846171410331, -2.941650167909708458, 5.493944474033886749 ) ) ;
#16958 = CARTESIAN_POINT ( 'NONE',  ( 1.754713504580569960, -0.04894067796610205440, 3.634325740584615883 ) ) ;
#16959 = CARTESIAN_POINT ( 'NONE',  ( 2.180207327701309872, -0.3934322033898309812, 5.586116916730190063 ) ) ;
#16960 = CARTESIAN_POINT ( 'NONE',  ( -0.1749999999999999889, 2.700000000000000178, 1.600000000000000089 ) ) ;
#16961 = CARTESIAN_POINT ( 'NONE',  ( 11.62823001646920140, -1.891469695401499911E-14, -4.352074256530609852E-14 ) ) ;
#16962 = VERTEX_POINT ( 'NONE', #512 ) ;
#16963 = EDGE_CURVE ( 'NONE', #3787, #17050, #7468, .T. ) ;
#16964 = CARTESIAN_POINT ( 'NONE',  ( 0.06367493584606445656, -0.001483050847457929866, 2.649999999999998579 ) ) ;
#16965 = CARTESIAN_POINT ( 'NONE',  ( -0.5320716618283710675, -3.007674156414609890, 6.992519451207139802 ) ) ;
#16966 = EDGE_LOOP ( 'NONE', ( #4484, #9782, #5471, #12566 ) ) ;
#16967 = EDGE_CURVE ( 'NONE', #13610, #8454, #8939, .T. ) ;
#16968 = ORIENTED_EDGE ( 'NONE', *, *, #15821, .F. ) ;
#16969 = CARTESIAN_POINT ( 'NONE',  ( 1.286937324407709804, -2.010118636378180224, 2.729584305145181133 ) ) ;
#16970 = CARTESIAN_POINT ( 'NONE',  ( -1.128670402850159737, -5.470974576271190770, 7.101865548313641696 ) ) ;
#16971 = ORIENTED_EDGE ( 'NONE', *, *, #4537, .F. ) ;
#16972 = CARTESIAN_POINT ( 'NONE',  ( 1.000000000000000000, -5.599999999999999645, 5.100000000000000533 ) ) ;
#16973 = CARTESIAN_POINT ( 'NONE',  ( 0.8731223871105069367, -0.4290254237288141370, 6.558046933601105799 ) ) ;
#16974 = ORIENTED_EDGE ( 'NONE', *, *, #4407, .F. ) ;
#16975 = CARTESIAN_POINT ( 'NONE',  ( -0.1749999999999999889, 5.200000000000000178, 1.600000000000000089 ) ) ;
#16976 = LINE ( 'NONE', #17060, #514 ) ;
#16977 = DIRECTION ( 'NONE',  ( -1.480297366166869931E-15, -1.000000000000000000, 0.000000000000000000 ) ) ;
#16978 = CARTESIAN_POINT ( 'NONE',  ( 1.102492180652039577, -2.309025507765959606, 2.968118700883580541 ) ) ;
#16979 = CARTESIAN_POINT ( 'NONE',  ( 1.289999999999999813, 4.099999999999999645, 0.6000000000000067502 ) ) ;
#16980 = CARTESIAN_POINT ( 'NONE',  ( 2.484260633728970546, -0.3578389830508479363, 3.766563288620793593 ) ) ;
#16981 = ORIENTED_EDGE ( 'NONE', *, *, #8793, .F. ) ;
#16982 = FACE_OUTER_BOUND ( 'NONE', #17552, .T. ) ;
#16983 = ORIENTED_EDGE ( 'NONE', *, *, #15192, .T. ) ;
#16984 = CARTESIAN_POINT ( 'NONE',  ( -1.229686204202100175, -5.164643153926309793, 2.674737924334550154 ) ) ;
#16985 = CARTESIAN_POINT ( 'NONE',  ( 2.328217775191430139, -5.381991525423729605, 5.043379051721160522 ) ) ;
#16986 = ORIENTED_EDGE ( 'NONE', *, *, #14183, .T. ) ;
#16987 = EDGE_CURVE ( 'NONE', #11273, #15567, #11715, .T. ) ;
#16988 = CARTESIAN_POINT ( 'NONE',  ( 2.353194804772640314, -0.07563559322033941434, 4.731327187377229571 ) ) ;
#16989 = CARTESIAN_POINT ( 'NONE',  ( -0.3743405594629430344, -5.457627118644070130, 7.023440622744399953 ) ) ;
#16990 = LINE ( 'NONE', #15446, #12921 ) ;
#16991 = ORIENTED_EDGE ( 'NONE', *, *, #11183, .T. ) ;
#16992 = DIRECTION ( 'NONE',  ( -1.000000000000000000, -1.734723475976809806E-16, -1.110223024625159992E-16 ) ) ;
#16993 = CARTESIAN_POINT ( 'NONE',  ( -2.260890494820599894, -1.544352870612419881, 4.046455925041199997 ) ) ;
#16994 = DIRECTION ( 'NONE',  ( -1.110223024625159992E-16, 1.000000000000000000, 0.000000000000000000 ) ) ;
#16995 = CARTESIAN_POINT ( 'NONE',  ( 1.423520578776751533, -2.056695212954759100, 3.220645071516909930 ) ) ;
#16996 = DIRECTION ( 'NONE',  ( 0.000000000000000000, 0.000000000000000000, 1.000000000000000000 ) ) ;
#16997 = ORIENTED_EDGE ( 'NONE', *, *, #8015, .F. ) ;
#16998 = DIRECTION ( 'NONE',  ( 1.224646799147350002E-16, -1.000000000000000000, -6.123233995736769734E-17 ) ) ;
#16999 = CARTESIAN_POINT ( 'NONE',  ( 2.638803263991410741, -0.08008474576271243373, 4.982085668537405532 ) ) ;
#17000 = CARTESIAN_POINT ( 'NONE',  ( -0.2620510901103649815, -3.706322805063249959, 2.361180871966390260 ) ) ;
#17001 = DIRECTION ( 'NONE',  ( -4.177994306516050823E-17, 0.7310552682428690385, -0.6823182503600111470 ) ) ;
#17002 = DIRECTION ( 'NONE',  ( -1.000000000000000000, 0.000000000000000000, 0.000000000000000000 ) ) ;
#17003 = CARTESIAN_POINT ( 'NONE',  ( -0.08231150243516484333, -5.298516949152545230, 2.050000000000001155 ) ) ;
#17004 = ORIENTED_EDGE ( 'NONE', *, *, #4833, .T. ) ;
#17005 = ORIENTED_EDGE ( 'NONE', *, *, #15827, .T. ) ;
#17006 = DIRECTION ( 'NONE',  ( 1.000000000000000000, -5.363760801114599979E-16, 0.000000000000000000 ) ) ;
#17007 = AXIS2_PLACEMENT_3D ( 'NONE', #7636, #6416, #17599 ) ;
#17008 = CARTESIAN_POINT ( 'NONE',  ( 1.899999999999999911, 2.000000000000000000, 1.600000000000000089 ) ) ;
#17009 = CARTESIAN_POINT ( 'NONE',  ( -1.399999999999999911, 0.5999999999999999778, 6.100000000000000533 ) ) ;
#17010 = ORIENTED_EDGE ( 'NONE', *, *, #12357, .F. ) ;
#17011 = CARTESIAN_POINT ( 'NONE',  ( 1.864786684738361178, -0.7952867690272195089, 2.817120744449660652 ) ) ;
#17012 = LINE ( 'NONE', #12775, #10256 ) ;
#17013 = CARTESIAN_POINT ( 'NONE',  ( 1.000000000000000000, -5.500000000000000000, 6.100000000000000533 ) ) ;
#17014 = CARTESIAN_POINT ( 'NONE',  ( 0.6864473529425539899, -1.008722239981789892, 6.951118770549889803 ) ) ;
#17015 = DIRECTION ( 'NONE',  ( 1.000000000000000000, 0.000000000000000000, 0.000000000000000000 ) ) ;
#17016 = CARTESIAN_POINT ( 'NONE',  ( -2.351999299633229956, -3.333710192450639820, 4.782734406438290620 ) ) ;
#17017 = DIRECTION ( 'NONE',  ( 0.000000000000000000, 0.000000000000000000, -1.000000000000000000 ) ) ;
#17018 = CARTESIAN_POINT ( 'NONE',  ( 1.831349212334668852, -4.009070552811004440, 3.772065786216904026 ) ) ;
#17019 = LINE ( 'NONE', #3130, #6146 ) ;
#17020 = ORIENTED_EDGE ( 'NONE', *, *, #12220, .F. ) ;
#17021 = CARTESIAN_POINT ( 'NONE',  ( -0.5500000000000000444, -2.399999999999999911, 3.299999999999999822 ) ) ;
#17022 = ORIENTED_EDGE ( 'NONE', *, *, #12648, .T. ) ;
#17023 = AXIS2_PLACEMENT_3D ( 'NONE', #978, #15920, #16433 ) ;
#17024 = FILL_AREA_STYLE ('',( #11565 ) ) ;
#17025 = ORIENTED_EDGE ( 'NONE', *, *, #6657, .T. ) ;
#17026 = CARTESIAN_POINT ( 'NONE',  ( -2.500000000000000000, 2.000000000000000000, 0.5999999999999999778 ) ) ;
#17027 = EDGE_LOOP ( 'NONE', ( #7876, #426, #10924, #11230 ) ) ;
#17028 = CARTESIAN_POINT ( 'NONE',  ( -2.046424002475610404, -5.228813559322024851, 4.536201610417774255 ) ) ;
#17029 = DIRECTION ( 'NONE',  ( 0.000000000000000000, 0.000000000000000000, 1.000000000000000000 ) ) ;
#17030 = CARTESIAN_POINT ( 'NONE',  ( 4.225031457058369810E-16, 2.299999999999999822, 7.700000000000000178 ) ) ;
#17031 = CARTESIAN_POINT ( 'NONE',  ( -1.899999999999999911, 2.799999999999999822, 1.600000000000000089 ) ) ;
#17032 = CARTESIAN_POINT ( 'NONE',  ( -1.385366411767399608, -5.164643153926310681, 2.415423146782709640 ) ) ;
#17033 = VECTOR ( 'NONE', #5183, 1000.000000000000000 ) ;
#17034 = PLANE ( 'NONE',  #511 ) ;
#17035 = CARTESIAN_POINT ( 'NONE',  ( 0.1749999999999999889, 7.500000000000000000, 3.100000000000000089 ) ) ;
#17036 = CARTESIAN_POINT ( 'NONE',  ( 2.075124426334590044, -2.681638120378570189, 5.810227140144509583 ) ) ;
#17037 = CARTESIAN_POINT ( 'NONE',  ( -1.959085573314230055, -2.964938456198001671, 5.313910057793616026 ) ) ;
#17038 = EDGE_CURVE ( 'NONE', #3716, #11589, #607, .T. ) ;
#17039 = CARTESIAN_POINT ( 'NONE',  ( -2.500000000000000000, 4.700000000000000178, 0.6099999999999999867 ) ) ;
#17040 = ADVANCED_FACE ( 'NONE', ( #10497 ), #16156, .T. ) ;
#17041 = AXIS2_PLACEMENT_3D ( 'NONE', #11299, #12866, #4436 ) ;
#17042 = ADVANCED_FACE ( 'NONE', ( #8522 ), #14172, .F. ) ;
#17043 = CARTESIAN_POINT ( 'NONE',  ( 1.850000000000000089, 0.7500000000000000000, 7.700000000000000178 ) ) ;
#17044 = ORIENTED_EDGE ( 'NONE', *, *, #12782, .T. ) ;
#17045 = CARTESIAN_POINT ( 'NONE',  ( -2.351526912647309953, -0.2269067796610169940, 4.606040641882809261 ) ) ;
#17046 = CARTESIAN_POINT ( 'NONE',  ( 2.301223891756920104, -2.611773255513699876, 5.193066210047949660 ) ) ;
#17047 = VERTEX_POINT ( 'NONE', #6616 ) ;
#17048 = AXIS2_PLACEMENT_3D ( 'NONE', #10364, #7685, #3330 ) ;
#17049 = AXIS2_PLACEMENT_3D ( 'NONE', #6349, #3768, #12013 ) ;
#17050 = VERTEX_POINT ( 'NONE', #12273 ) ;
#17051 = AXIS2_PLACEMENT_3D ( 'NONE', #13093, #411, #6050 ) ;
#17052 = CARTESIAN_POINT ( 'NONE',  ( 2.340959815966380031, -3.849893411152960354, 4.942183458383420991 ) ) ;
#17053 = DIRECTION ( 'NONE',  ( 1.000000000000000000, 0.000000000000000000, 0.000000000000000000 ) ) ;
#17054 = CARTESIAN_POINT ( 'NONE',  ( 2.586172839791708533, -5.364194915254235418, 4.104546363490930716 ) ) ;
#17055 = ORIENTED_EDGE ( 'NONE', *, *, #10868, .T. ) ;
#17056 = CARTESIAN_POINT ( 'NONE',  ( -1.795861365445549973, -0.5491525423728815802, 3.705232155007899930 ) ) ;
#17057 = ORIENTED_EDGE ( 'NONE', *, *, #11207, .F. ) ;
#17058 = EDGE_CURVE ( 'NONE', #5909, #268, #15632, .T. ) ;
#17059 = DIRECTION ( 'NONE',  ( -0.000000000000000000, 1.000000000000000000, 0.000000000000000000 ) ) ;
#17060 = CARTESIAN_POINT ( 'NONE',  ( -2.500000000000000000, 11.15000000000000036, 2.137972338849589826E-15 ) ) ;
#17061 = CARTESIAN_POINT ( 'NONE',  ( -0.9000000000000000222, 2.050000000000000266, 3.600000000000000089 ) ) ;
#17062 = CARTESIAN_POINT ( 'NONE',  ( -0.9123513484652393535, -2.052854336594789331, 2.860838000723768815 ) ) ;
#17063 = EDGE_CURVE ( 'NONE', #17390, #13613, #14866, .T. ) ;
#17064 = ORIENTED_EDGE ( 'NONE', *, *, #2379, .T. ) ;
#17065 = LINE ( 'NONE', #3096, #14282 ) ;
#17066 = VECTOR ( 'NONE', #14428, 1000.000000000000000 ) ;
#17067 = ADVANCED_FACE ( 'NONE', ( #787 ), #9106, .F. ) ;
#17068 = CARTESIAN_POINT ( 'NONE',  ( 8.549934884138839976E-16, 6.262741699796950279, 5.100000000000000533 ) ) ;
#17069 = ORIENTED_EDGE ( 'NONE', *, *, #6755, .F. ) ;
#17070 = AXIS2_PLACEMENT_3D ( 'NONE', #2986, #17029, #109 ) ;
#17071 = CARTESIAN_POINT ( 'NONE',  ( -1.899999999999999911, 11.25000000000000000, 7.649999999999999467 ) ) ;
#17072 = CARTESIAN_POINT ( 'NONE',  ( -0.3803919826357066158, -5.591101694915256104, 2.682580100125310896 ) ) ;
#17073 = AXIS2_PLACEMENT_3D ( 'NONE', #3275, #11691, #2157 ) ;
#17074 = CARTESIAN_POINT ( 'NONE',  ( 1.978267656359408821, -0.1023305084745769755, 5.974740860598791947 ) ) ;
#17075 = DIRECTION ( 'NONE',  ( -1.000000000000000000, 0.000000000000000000, 0.000000000000000000 ) ) ;
#17076 = ORIENTED_EDGE ( 'NONE', *, *, #16662, .F. ) ;
#17077 = CARTESIAN_POINT ( 'NONE',  ( -0.5999999999999999778, 10.80000000000000071, 7.700000000000000178 ) ) ;
#17078 = CARTESIAN_POINT ( 'NONE',  ( 2.349464193210359930, -2.243001519261070165, 4.563019372514570016 ) ) ;
#17079 = CARTESIAN_POINT ( 'NONE',  ( -2.500000000000000000, 8.500000000000000000, 0.6099999999999999867 ) ) ;
#17080 = CARTESIAN_POINT ( 'NONE',  ( -1.058024172752510594, -1.730659176918718956, 2.940600473883360433 ) ) ;
#17081 = VECTOR ( 'NONE', #4888, 1000.000000000000000 ) ;
#17082 = VECTOR ( 'NONE', #8770, 1000.000000000000000 ) ;
#17084 = EDGE_CURVE ( 'NONE', #14807, #17218, #3456, .T. ) ;
#17083 = CARTESIAN_POINT ( 'NONE',  ( 1.899999999999999911, 11.25000000000000000, 7.649999999999999467 ) ) ;
#17085 = EDGE_LOOP ( 'NONE', ( #9734, #4609, #3185, #9023 ) ) ;
#17086 = AXIS2_PLACEMENT_3D ( 'NONE', #8097, #13737, #6795 ) ;
#17087 = CARTESIAN_POINT ( 'NONE',  ( 1.899999999999999911, 0.7211102550927970256, 7.649999999999999467 ) ) ;
#17088 = CARTESIAN_POINT ( 'NONE',  ( -2.650076489488250697, -0.5224576271186435195, 4.841243018609314497 ) ) ;
#17089 = CARTESIAN_POINT ( 'NONE',  ( 0.6150581927482109412, -4.451548030288480895, 6.971662190339319665 ) ) ;
#17090 = CARTESIAN_POINT ( 'NONE',  ( 3.179896940101190659E-17, 3.786446520921940007, 7.919316580472860245 ) ) ;
#17091 = DIRECTION ( 'NONE',  ( -1.000000000000000000, 0.000000000000000000, 6.123233995736769734E-17 ) ) ;
#17092 = CARTESIAN_POINT ( 'NONE',  ( 2.234315482767910144, -5.059745762711860273, 3.960850823455320580 ) ) ;
#17093 = ORIENTED_EDGE ( 'NONE', *, *, #11410, .T. ) ;
#17094 = EDGE_LOOP ( 'NONE', ( #3015, #9521, #1563, #3517 ) ) ;
#17095 = PLANE ( 'NONE',  #10359 ) ;
#17096 = VECTOR ( 'NONE', #15788, 1000.000000000000000 ) ;
#17097 = CARTESIAN_POINT ( 'NONE',  ( 1.250000000000000000, 0.5999999999999999778, 7.599999999999999645 ) ) ;
#17098 = VECTOR ( 'NONE', #9089, 1000.000000000000000 ) ;
#17099 = EDGE_LOOP ( 'NONE', ( #14978, #17134, #9683, #3398 ) ) ;
#17100 = EDGE_CURVE ( 'NONE', #15477, #18021, #2080, .T. ) ;
#17101 = CARTESIAN_POINT ( 'NONE',  ( 2.516451517878131927, -0.9117282104686613708, 3.857037693030633818 ) ) ;
#17102 = EDGE_CURVE ( 'NONE', #6472, #12303, #7733, .T. ) ;
#17103 = CARTESIAN_POINT ( 'NONE',  ( 1.882879255550339082, -0.4963798976394455664, 2.835213315261639000 ) ) ;
#17104 = CARTESIAN_POINT ( 'NONE',  ( -1.750000000000000000, 0.5999999999999999778, 7.700000000000000178 ) ) ;
#17105 = CARTESIAN_POINT ( 'NONE',  ( 2.349464193210359930, -2.243001519261070165, 4.563019372514570016 ) ) ;
#17107 = EDGE_CURVE ( 'NONE', #16021, #9457, #5338, .T. ) ;
#17106 = DIRECTION ( 'NONE',  ( 0.000000000000000000, -1.000000000000000000, 0.000000000000000000 ) ) ;
#17108 = CARTESIAN_POINT ( 'NONE',  ( 1.866416942370620058, -3.962493976234419790, 3.266391446483460026 ) ) ;
#17109 = AXIS2_PLACEMENT_3D ( 'NONE', #15066, #6325, #9199 ) ;
#17110 = DIRECTION ( 'NONE',  ( 0.000000000000000000, -1.000000000000000000, 0.000000000000000000 ) ) ;
#17111 = CARTESIAN_POINT ( 'NONE',  ( -2.500000000000000000, 4.700000000000000178, 0.6099999999999999867 ) ) ;
#17112 = DIRECTION ( 'NONE',  ( 0.000000000000000000, -1.000000000000000000, 0.000000000000000000 ) ) ;
#17113 = EDGE_LOOP ( 'NONE', ( #6469, #8379, #12192, #16742 ) ) ;
#17114 = PLANE ( 'NONE',  #1608 ) ;
#17115 = VERTEX_POINT ( 'NONE', #16342 ) ;
#17116 = CARTESIAN_POINT ( 'NONE',  ( 1.000000000000000000, 6.799999999999999822, 7.700000000000000178 ) ) ;
#17117 = CARTESIAN_POINT ( 'NONE',  ( 1.875000000000000000, -2.296212748401290437E-16, 8.300000000000000711 ) ) ;
#17118 = ORIENTED_EDGE ( 'NONE', *, *, #4307, .F. ) ;
#17119 = VECTOR ( 'NONE', #1161, 1000.000000000000000 ) ;
#17120 = CARTESIAN_POINT ( 'NONE',  ( -1.725722849164588624, -5.497669491525425833, 5.812007984777676661 ) ) ;
#17121 = CARTESIAN_POINT ( 'NONE',  ( -1.630703155447540631, -3.267686203945749490, 2.606218513833090000 ) ) ;
#17122 = LINE ( 'NONE', #2617, #4636 ) ;
#17123 = ADVANCED_FACE ( 'NONE', ( #15155 ), #979, .T. ) ;
#17124 = DIRECTION ( 'NONE',  ( -1.000000000000000000, 0.000000000000000000, 0.000000000000000000 ) ) ;
#17125 = CARTESIAN_POINT ( 'NONE',  ( -0.9138909625329535436, -4.911779243796845051, 2.204775695797560164 ) ) ;
#17126 = LINE ( 'NONE', #8712, #10262 ) ;
#17127 = CARTESIAN_POINT ( 'NONE',  ( -0.4000000000000000222, 2.399999999999999911, 6.100000000000000533 ) ) ;
#17128 = CARTESIAN_POINT ( 'NONE',  ( 1.764807890102179977, -2.378890372630820149, 3.143016121304719857 ) ) ;
#17129 = CARTESIAN_POINT ( 'NONE',  ( 1.883235269974540937, -2.359442960702510472, 5.517512544583896172 ) ) ;
#17130 = CARTESIAN_POINT ( 'NONE',  ( 0.004026115436751699292, -5.086189479527880586, 2.487698411374999807 ) ) ;
#17131 = VECTOR ( 'NONE', #13608, 1000.000000000000000 ) ;
#17132 = ADVANCED_FACE ( 'NONE', ( #6328 ), #3646, .T. ) ;
#17133 = LINE ( 'NONE', #5767, #8858 ) ;
#17134 = ORIENTED_EDGE ( 'NONE', *, *, #2682, .T. ) ;
#17135 = CARTESIAN_POINT ( 'NONE',  ( -2.350067830300900162, -0.2224576271186440024, 4.825253242917699303 ) ) ;
#17136 = CARTESIAN_POINT ( 'NONE',  ( -2.182690844914350059, -1.680241723982170088, 5.580117243900479806 ) ) ;
#17137 = ORIENTED_EDGE ( 'NONE', *, *, #3511, .T. ) ;
#17138 = LINE ( 'NONE', #15773, #3789 ) ;
#17139 = ORIENTED_EDGE ( 'NONE', *, *, #12418, .T. ) ;
#17140 = CARTESIAN_POINT ( 'NONE',  ( -2.211317922628891264, -3.127956474216019966, 3.894507149290469705 ) ) ;
#17141 = CARTESIAN_POINT ( 'NONE',  ( 2.519547246525509543, -5.059745762711855832, 3.866491354109194756 ) ) ;
#17142 = ORIENTED_EDGE ( 'NONE', *, *, #2594, .F. ) ;
#17143 = EDGE_CURVE ( 'NONE', #17417, #8570, #11992, .T. ) ;
#17144 = CIRCLE ( 'NONE', #10347, 0.2500000000000006106 ) ;
#17145 = CARTESIAN_POINT ( 'NONE',  ( 0.4360591020457930123, -0.3088983050847460277, 2.387347919655840034 ) ) ;
#17146 = ORIENTED_EDGE ( 'NONE', *, *, #13021, .F. ) ;
#17147 = LINE ( 'NONE', #5697, #2861 ) ;
#17148 = DIRECTION ( 'NONE',  ( 9.654113257610059070E-17, 0.000000000000000000, 1.000000000000000000 ) ) ;
#17149 = CARTESIAN_POINT ( 'NONE',  ( 0.8493734496528324573, -2.844656138396588929, 6.569081749323157915 ) ) ;
#17150 = VERTEX_POINT ( 'NONE', #5233 ) ;
#17151 = CARTESIAN_POINT ( 'NONE',  ( 0.5500000000000000444, 6.450000000000000178, 3.399999999999999911 ) ) ;
#17152 = DIRECTION ( 'NONE',  ( -1.000000000000000000, 1.480297366166879989E-15, 0.000000000000000000 ) ) ;
#17153 = EDGE_CURVE ( 'NONE', #16560, #2052, #2181, .T. ) ;
#17154 = VERTEX_POINT ( 'NONE', #13469 ) ;
#17155 = AXIS2_PLACEMENT_3D ( 'NONE', #335, #10137, #8847 ) ;
#17156 = LINE ( 'NONE', #6052, #16870 ) ;
#17157 = CARTESIAN_POINT ( 'NONE',  ( 1.925796468768800063, -5.404237288135590234, 6.052706598917719560 ) ) ;
#17158 = DIRECTION ( 'NONE',  ( -1.000000000000000000, 0.000000000000000000, 0.000000000000000000 ) ) ;
#17159 = EDGE_CURVE ( 'NONE', #2376, #10505, #4945, .T. ) ;
#17160 = CARTESIAN_POINT ( 'NONE',  ( -2.328217775191430139, -0.2180084745762720932, 5.043379051721168516 ) ) ;
#17161 = DIRECTION ( 'NONE',  ( -1.000000000000000000, 0.000000000000000000, 0.000000000000000000 ) ) ;
#17162 = EDGE_CURVE ( 'NONE', #5409, #14832, #10287, .T. ) ;
#17163 = ADVANCED_FACE ( 'NONE', ( #6423 ), #5138, .F. ) ;
#17164 = VERTEX_POINT ( 'NONE', #5044 ) ;
#17165 = CARTESIAN_POINT ( 'NONE',  ( 0.9000000000000000222, 6.450000000000000178, 3.600000000000000089 ) ) ;
#17166 = EDGE_CURVE ( 'NONE', #1884, #15033, #12666, .T. ) ;
#17167 = CARTESIAN_POINT ( 'NONE',  ( -0.1824815401349519917, -1.101875393134939873, 7.046368721022739479 ) ) ;
#17168 = ADVANCED_FACE ( 'NONE', ( #16434 ), #9402, .T. ) ;
#17169 = DIRECTION ( 'NONE',  ( 3.670158759091429763E-17, 0.000000000000000000, 1.000000000000000000 ) ) ;
#17170 = CARTESIAN_POINT ( 'NONE',  ( 2.049636678546640667, -2.243001519261071053, 4.582138519505345009 ) ) ;
#17171 = PLANE ( 'NONE',  #1709 ) ;
#17172 = ORIENTED_EDGE ( 'NONE', *, *, #10277, .T. ) ;
#17173 = PLANE ( 'NONE',  #15357 ) ;
#17174 = CARTESIAN_POINT ( 'NONE',  ( 0.9664230948141925293, -0.01779661016949178609, 2.228384861502251457 ) ) ;
#17175 = CARTESIAN_POINT ( 'NONE',  ( -2.033393610350109793, -4.777584066324510381, 5.884928737465370041 ) ) ;
#17176 = PLANE ( 'NONE',  #16953 ) ;
#17177 = CARTESIAN_POINT ( 'NONE',  ( 0.2335786437626899970, 3.050000000000000266, 1.958578643762689753 ) ) ;
#17178 = CARTESIAN_POINT ( 'NONE',  ( 2.155845792290829621, -5.055296610169490279, 3.756158857535770057 ) ) ;
#17179 = VERTEX_POINT ( 'NONE', #9584 ) ;
#17180 = ORIENTED_EDGE ( 'NONE', *, *, #11743, .T. ) ;
#17181 = CARTESIAN_POINT ( 'NONE',  ( 0.6914213562373080491, 6.450000000000000178, 2.557842712474620139 ) ) ;
#17182 = DIRECTION ( 'NONE',  ( 0.7071067811865480168, 0.000000000000000000, -0.7071067811865470176 ) ) ;
#17183 = EDGE_CURVE ( 'NONE', #12747, #13413, #139, .T. ) ;
#17184 = ORIENTED_EDGE ( 'NONE', *, *, #9286, .F. ) ;
#17185 = CARTESIAN_POINT ( 'NONE',  ( 1.853635285637830865, -1.191187669928120529, 6.599249831075482575 ) ) ;
#17186 = FACE_OUTER_BOUND ( 'NONE', #13527, .T. ) ;
#17187 = CARTESIAN_POINT ( 'NONE',  ( 0.5500000000000000444, 7.799999999999999822, 1.600000000000000089 ) ) ;
#17188 = CARTESIAN_POINT ( 'NONE',  ( -0.1226612266410539998, -2.662190708450249854, 7.050255286338659388 ) ) ;
#17189 = DIRECTION ( 'NONE',  ( 1.110223024625159992E-16, 0.000000000000000000, -1.000000000000000000 ) ) ;
#17190 = CARTESIAN_POINT ( 'NONE',  ( 2.316126390218360420, -0.8651516338920848259, 3.404364157709320438 ) ) ;
#17191 = FACE_OUTER_BOUND ( 'NONE', #7053, .T. ) ;
#17192 = CARTESIAN_POINT ( 'NONE',  ( -1.503462833636818541, -5.095857339597785973, 3.304888304972901647 ) ) ;
#17193 = CARTESIAN_POINT ( 'NONE',  ( 1.889999999999999902, 3.500000000000000000, 0.5999999999999999778 ) ) ;
#17194 = DIRECTION ( 'NONE',  ( -1.850371707708589879E-16, -1.000000000000000000, 0.000000000000000000 ) ) ;
#17195 = ORIENTED_EDGE ( 'NONE', *, *, #11912, .F. ) ;
#17196 = EDGE_LOOP ( 'NONE', ( #3771, #14003, #15436, #6011 ) ) ;
#17197 = DIRECTION ( 'NONE',  ( -1.000000000000000000, 0.000000000000000000, 1.142385477618690234E-14 ) ) ;
#17198 = ADVANCED_FACE ( 'NONE', ( #2830 ), #5787, .F. ) ;
#17199 = ORIENTED_EDGE ( 'NONE', *, *, #7338, .F. ) ;
#17200 = AXIS2_PLACEMENT_3D ( 'NONE', #17234, #9953, #7452 ) ;
#17201 = CARTESIAN_POINT ( 'NONE',  ( 1.949083719010301197, -5.359745762711870753, 4.055210292801453953 ) ) ;
#17202 = CARTESIAN_POINT ( 'NONE',  ( -0.7540633504678314614, -3.360839357098899693, 2.155495695330209127 ) ) ;
#17203 = FACE_OUTER_BOUND ( 'NONE', #11995, .T. ) ;
#17204 = DIRECTION ( 'NONE',  ( -3.172065784643300034E-16, 1.000000000000000000, 0.000000000000000000 ) ) ;
#17205 = CARTESIAN_POINT ( 'NONE',  ( -2.220446049250309876E-16, -9.868649107779171166E-17, 1.600000000000000089 ) ) ;
#17206 = CARTESIAN_POINT ( 'NONE',  ( 1.936998685628529948, -0.8418633456037969420, 3.363294429306519895 ) ) ;
#17207 = LINE ( 'NONE', #3149, #17679 ) ;
#17208 = CARTESIAN_POINT ( 'NONE',  ( 0.1226612266411070129, -2.937809291549740021, 7.050255286338659388 ) ) ;
#17209 = CARTESIAN_POINT ( 'NONE',  ( 0.8735826871841618768, -4.106064582324130185, 6.557889967484662463 ) ) ;
#17210 = CARTESIAN_POINT ( 'NONE',  ( 1.921786527979010062, -0.05783898305084796132, 3.977907449687776431 ) ) ;
#17211 = VECTOR ( 'NONE', #1363, 1000.000000000000000 ) ;
#17212 = CARTESIAN_POINT ( 'NONE',  ( 1.899999999999999911, 11.15000000000000036, -6.992551034670250827E-16 ) ) ;
#17213 = DIRECTION ( 'NONE',  ( -1.233581138472399909E-16, 1.000000000000000000, 6.167905692361979821E-17 ) ) ;
#17214 = ORIENTED_EDGE ( 'NONE', *, *, #6108, .F. ) ;
#17215 = CARTESIAN_POINT ( 'NONE',  ( -0.5606293434988356417, -4.269082600342137823, 7.293994686233948421 ) ) ;
#17216 = CARTESIAN_POINT ( 'NONE',  ( 2.052786957354850728, -0.07563559322033948373, 4.727327971967373976 ) ) ;
#17217 = CARTESIAN_POINT ( 'NONE',  ( 1.962536940652990003, -2.704926408666860294, 5.998920491814760503 ) ) ;
#17218 = VERTEX_POINT ( 'NONE', #2929 ) ;
#17219 = ORIENTED_EDGE ( 'NONE', *, *, #14906, .T. ) ;
#17220 = CARTESIAN_POINT ( 'NONE',  ( 1.981271652668328720, -3.966334852594400662, 5.970160748022401265 ) ) ;
#17221 = DIRECTION ( 'NONE',  ( 1.000000000000000000, 0.000000000000000000, 0.000000000000000000 ) ) ;
#17222 = CARTESIAN_POINT ( 'NONE',  ( -2.540842781840720654, -5.211016949152535993, 5.466141598148674952 ) ) ;
#17223 = PLANE ( 'NONE',  #9739 ) ;
#17224 = ORIENTED_EDGE ( 'NONE', *, *, #8684, .F. ) ;
#17225 = VECTOR ( 'NONE', #7934, 1000.000000000000000 ) ;
#17226 = CARTESIAN_POINT ( 'NONE',  ( 0.5999999999999999778, -7.347880794884110368E-17, 7.599999999999999645 ) ) ;
#17227 = CARTESIAN_POINT ( 'NONE',  ( -2.286166334984490067, -0.5135593220338989795, 5.258525443163870605 ) ) ;
#17228 = ORIENTED_EDGE ( 'NONE', *, *, #11975, .F. ) ;
#17229 = DIRECTION ( 'NONE',  ( 0.7071067811865474617, 0.000000000000000000, -0.7071067811865474617 ) ) ;
#17230 = PLANE ( 'NONE',  #13571 ) ;
#17231 = CARTESIAN_POINT ( 'NONE',  ( -1.951270856817509003, -3.263845327585779277, 5.338313313320930398 ) ) ;
#17232 = CARTESIAN_POINT ( 'NONE',  ( 2.614198783383141045, -0.3667372881355940861, 4.243032045539284702 ) ) ;
#17233 = ORIENTED_EDGE ( 'NONE', *, *, #324, .F. ) ;
#17234 = CARTESIAN_POINT ( 'NONE',  ( 1.800000000000000044, 11.40000000000000036, 1.600000000000000089 ) ) ;
#17235 = DIRECTION ( 'NONE',  ( 0.000000000000000000, 0.000000000000000000, 1.000000000000000000 ) ) ;
#17236 = CARTESIAN_POINT ( 'NONE',  ( 1.489797906646480596, -0.4112288135593234473, 6.112509577910826941 ) ) ;
#17237 = LINE ( 'NONE', #16117, #14671 ) ;
#17238 = ORIENTED_EDGE ( 'NONE', *, *, #7167, .F. ) ;
#17239 = CARTESIAN_POINT ( 'NONE',  ( -2.012177589105470066, -5.515466101694915579, 5.107213040360599088 ) ) ;
#17240 = SURFACE_STYLE_FILL_AREA ( #4559 ) ;
#17241 = CARTESIAN_POINT ( 'NONE',  ( -2.058670345754649134, -0.2491525423728820077, 3.559656372813929881 ) ) ;
#17242 = CARTESIAN_POINT ( 'NONE',  ( -0.5058614788087384406, -0.2909039927201511055, 2.084176093893880921 ) ) ;
#17243 = CARTESIAN_POINT ( 'NONE',  ( -0.5355577887185811736, -4.567989471729919870, 7.299286738308172318 ) ) ;
#17244 = ORIENTED_EDGE ( 'NONE', *, *, #5000, .T. ) ;
#17245 = PRESENTATION_LAYER_ASSIGNMENT (  '', '', ( #8692 ) ) ;
#17246 = CARTESIAN_POINT ( 'NONE',  ( 1.777964140657680048, -0.8689925102520590361, 6.241943319976220650 ) ) ;
#17247 = CARTESIAN_POINT ( 'NONE',  ( -0.1749999999999999889, 4.299999999999999822, 1.600000000000000089 ) ) ;
#17248 = CARTESIAN_POINT ( 'NONE',  ( 1.313542260532459149, -2.475884402143949892, 6.277817661335856059 ) ) ;
#17249 = FACE_OUTER_BOUND ( 'NONE', #13353, .T. ) ;
#17250 = ADVANCED_FACE ( 'NONE', ( #16982 ), #8476, .T. ) ;
#17251 = CARTESIAN_POINT ( 'NONE',  ( -1.850000000000000089, 0.7500000000000000000, 8.300000000000000711 ) ) ;
#17252 = EDGE_LOOP ( 'NONE', ( #3829, #6382, #12849, #15836 ) ) ;
#17253 = EDGE_CURVE ( 'NONE', #10426, #17808, #4668, .T. ) ;
#17254 = FACE_OUTER_BOUND ( 'NONE', #4955, .T. ) ;
#17255 = CARTESIAN_POINT ( 'NONE',  ( 2.159308672244681482, -0.8457042219637719294, 6.242886823772496818 ) ) ;
#17256 = ADVANCED_FACE ( 'NONE', ( #11255 ), #16804, .F. ) ;
#17257 = CARTESIAN_POINT ( 'NONE',  ( -2.065623031241579977, -5.033755237495680213, 3.572193642975310279 ) ) ;
#17258 = LINE ( 'NONE', #10231, #9569 ) ;
#17259 = ADVANCED_FACE ( 'NONE', ( #9956 ), #14025, .F. ) ;
#17260 = FACE_OUTER_BOUND ( 'NONE', #4472, .T. ) ;
#17261 = ORIENTED_EDGE ( 'NONE', *, *, #11357, .T. ) ;
#17262 = ORIENTED_EDGE ( 'NONE', *, *, #7123, .F. ) ;
#17263 = CARTESIAN_POINT ( 'NONE',  ( -1.149999999999999911, 6.472933199251450276, 6.846017351831609865 ) ) ;
#17264 = DIRECTION ( 'NONE',  ( -1.110223024625159992E-16, 0.000000000000000000, -1.000000000000000000 ) ) ;
#17265 = VERTEX_POINT ( 'NONE', #8199 ) ;
#17266 = DIRECTION ( 'NONE',  ( 1.224646799147350002E-16, -1.000000000000000000, -6.123233995736769734E-17 ) ) ;
#17267 = CARTESIAN_POINT ( 'NONE',  ( 0.1749999999999999889, 5.200000000000000178, 1.600000000000000089 ) ) ;
#17268 = DIRECTION ( 'NONE',  ( -1.000000000000000000, 0.000000000000000000, 0.000000000000000000 ) ) ;
#17269 = CARTESIAN_POINT ( 'NONE',  ( -1.991984774470509922, -1.614217735477279980, 3.446707398186049875 ) ) ;
#17270 = CARTESIAN_POINT ( 'NONE',  ( 1.534924416212170017, -5.333856471232000018, 2.911460733964629899 ) ) ;
#17271 = ADVANCED_FACE ( 'NONE', ( #9775 ), #11062, .F. ) ;
#17272 = CARTESIAN_POINT ( 'NONE',  ( -1.670747221194380128, -5.103620102360550526, 3.047345349617600174 ) ) ;
#17273 = DIRECTION ( 'NONE',  ( 1.000000000000000000, -1.480297366166879989E-15, -1.850371707708599740E-16 ) ) ;
#17274 = CARTESIAN_POINT ( 'NONE',  ( 2.053221424930760097, -0.8651516338920849369, 3.549770689668250157 ) ) ;
#17275 = EDGE_CURVE ( 'NONE', #9237, #13339, #12362, .T. ) ;
#17276 = CARTESIAN_POINT ( 'NONE',  ( 2.500000000000000000, 4.700000000000000178, 0.5999999999999999778 ) ) ;
#17277 = CARTESIAN_POINT ( 'NONE',  ( 1.983927814618709873E-15, 10.80000000000000071, 8.599999999999999645 ) ) ;
#17278 = ORIENTED_EDGE ( 'NONE', *, *, #12998, .T. ) ;
#17279 = DIRECTION ( 'NONE',  ( -0.7071067811865470176, -0.7071067811865480168, 0.000000000000000000 ) ) ;
#17280 = ORIENTED_EDGE ( 'NONE', *, *, #4038, .F. ) ;
#17281 = DIRECTION ( 'NONE',  ( -3.700743415417190309E-15, 0.000000000000000000, -1.000000000000000000 ) ) ;
#17282 = LINE ( 'NONE', #12965, #10907 ) ;
#17283 = ORIENTED_EDGE ( 'NONE', *, *, #8391, .F. ) ;
#17284 = CARTESIAN_POINT ( 'NONE',  ( 1.679950111053631900, -5.404237288135596451, 5.880020650119711867 ) ) ;
#17285 = LINE ( 'NONE', #15939, #3813 ) ;
#17286 = DIRECTION ( 'NONE',  ( 2.220446049250319983E-16, 1.000000000000000000, -2.047034224795619731E-16 ) ) ;
#17287 = CARTESIAN_POINT ( 'NONE',  ( -0.6265155281652096120, -2.708767285026830951, 7.278874170247493502 ) ) ;
#17288 = SURFACE_STYLE_FILL_AREA ( #17394 ) ;
#17289 = CARTESIAN_POINT ( 'NONE',  ( 2.350000000000000089, -6.000000000000000000, 2.799999999999999822 ) ) ;
#17290 = LINE ( 'NONE', #16110, #2871 ) ;
#17291 = CARTESIAN_POINT ( 'NONE',  ( -1.899999999999999911, 10.00000000000000000, 7.286648454926749993E-16 ) ) ;
#17292 = CARTESIAN_POINT ( 'NONE',  ( -1.399999999999999911, -5.500000000000000000, 5.100000000000000533 ) ) ;
#17293 = CARTESIAN_POINT ( 'NONE',  ( -2.135041058613629694, -4.800872354612799597, 5.690123914223820023 ) ) ;
#17294 = CARTESIAN_POINT ( 'NONE',  ( -1.998374131852739266, -4.664983501243040287, 4.229465546630535755 ) ) ;
#17295 = CIRCLE ( 'NONE', #11421, 0.5000000000000000000 ) ;
#17296 = ADVANCED_FACE ( 'NONE', ( #13846 ), #1167, .F. ) ;
#17297 = CARTESIAN_POINT ( 'NONE',  ( -0.007508403481304109714, -5.269001837275429700, 2.444053578789410430 ) ) ;
#17298 = LINE ( 'NONE', #10187, #3230 ) ;
#17299 = EDGE_LOOP ( 'NONE', ( #3545, #124, #3163, #11599 ) ) ;
#17300 = CARTESIAN_POINT ( 'NONE',  ( 0.7137241095604313079, -3.500569086828633658, 2.143887406933319362 ) ) ;
#17301 = CARTESIAN_POINT ( 'NONE',  ( -1.994315313497099229, -0.2135593220338991571, 5.187224322759965922 ) ) ;
#17302 = CARTESIAN_POINT ( 'NONE',  ( 2.352760675243219968, -2.565196678937129882, 4.757121734156020132 ) ) ;
#17303 = ORIENTED_EDGE ( 'NONE', *, *, #17581, .T. ) ;
#17304 = VERTEX_POINT ( 'NONE', #1255 ) ;
#17305 = EDGE_CURVE ( 'NONE', #5781, #12188, #14131, .T. ) ;
#17306 = CARTESIAN_POINT ( 'NONE',  ( -4.440892098500630106E-16, -1.399999999999999911, 6.100000000000000533 ) ) ;
#17307 = ORIENTED_EDGE ( 'NONE', *, *, #4273, .T. ) ;
#17308 = VECTOR ( 'NONE', #7160, 1000.000000000000000 ) ;
#17309 = CARTESIAN_POINT ( 'NONE',  ( 1.854177340199709478, -3.989623140882689434, 6.149404042554680316 ) ) ;
#17310 = DIRECTION ( 'NONE',  ( 0.000000000000000000, 0.000000000000000000, 1.000000000000000000 ) ) ;
#17311 = CARTESIAN_POINT ( 'NONE',  ( -2.230812463554230352, -5.197669491525426011, 6.137473736419926773 ) ) ;
#17312 = VECTOR ( 'NONE', #5231, 1000.000000000000000 ) ;
#17313 = EDGE_LOOP ( 'NONE', ( #16587, #14938, #10481, #10084 ) ) ;
#17314 = VECTOR ( 'NONE', #9097, 1000.000000000000000 ) ;
#17315 = DIRECTION ( 'NONE',  ( -1.445602896647339508E-15, 0.000000000000000000, 1.000000000000000000 ) ) ;
#17316 = CARTESIAN_POINT ( 'NONE',  ( -0.4974685680287780354, -0.4601694915254240237, 7.000224381598740386 ) ) ;
#17317 = ORIENTED_EDGE ( 'NONE', *, *, #16967, .F. ) ;
#17318 = DIRECTION ( 'NONE',  ( -1.000000000000000000, -1.644774851296529842E-16, -1.110223024625159992E-16 ) ) ;
#17319 = DIRECTION ( 'NONE',  ( 1.554023113895890109E-14, -1.000000000000000000, -1.110223024626929998E-16 ) ) ;
#17320 = CARTESIAN_POINT ( 'NONE',  ( -1.899999999999999911, 2.799999999999999822, 0.5999999999999999778 ) ) ;
#17321 = CARTESIAN_POINT ( 'NONE',  ( -0.2739924515130059968, -2.984385868126320673, 6.734657214162127481 ) ) ;
#17322 = CARTESIAN_POINT ( 'NONE',  ( 2.653602652190420574, -0.07563559322033948373, 4.735326402787084277 ) ) ;
#17323 = EDGE_CURVE ( 'NONE', #14318, #240, #16706, .T. ) ;
#17324 = ORIENTED_EDGE ( 'NONE', *, *, #6543, .F. ) ;
#17325 = CARTESIAN_POINT ( 'NONE',  ( -1.670747221194377685, -5.103620102360557631, 3.047345349617607724 ) ) ;
#17326 = CARTESIAN_POINT ( 'NONE',  ( -1.000000000000000000, -6.000000000000000000, 5.100000000000000533 ) ) ;
#17327 = CLOSED_SHELL ( 'NONE', ( #4564, #8351, #16381, #1983, #12315, #3256, #9631, #17594, #12479, #13324, #9007, #5388, #10063, #3941, #16087, #17884, #5855, #13924, #934, #16389 ) ) ;
#17328 = AXIS2_PLACEMENT_3D ( 'NONE', #14431, #8778, #10250 ) ;
#17329 = ORIENTED_EDGE ( 'NONE', *, *, #7284, .T. ) ;
#17330 = AXIS2_PLACEMENT_3D ( 'NONE', #10443, #9147, #16104 ) ;
#17331 = CARTESIAN_POINT ( 'NONE',  ( 2.500000000000000000, 2.799999999999999822, 0.6099999999999999867 ) ) ;
#17332 = CARTESIAN_POINT ( 'NONE',  ( 1.300961508564179914, -5.422033898305079092, 6.661123742937279602 ) ) ;
#17333 = CARTESIAN_POINT ( 'NONE',  ( -1.899999999999999911, 2.000000000000000000, 2.388061258337340122E-16 ) ) ;
#17334 = FACE_OUTER_BOUND ( 'NONE', #2339, .T. ) ;
#17335 = VECTOR ( 'NONE', #12752, 1000.000000000000000 ) ;
#17336 = CARTESIAN_POINT ( 'NONE',  ( 0.9250303514740658706, -3.822764246504686270, 2.212544966868020602 ) ) ;
#17337 = ORIENTED_EDGE ( 'NONE', *, *, #2803, .T. ) ;
#17338 = CARTESIAN_POINT ( 'NONE',  ( 1.332058588847409908, -2.499172690432239996, 6.640197310420189680 ) ) ;
#17339 = CARTESIAN_POINT ( 'NONE',  ( -1.899999999999999911, -2.607830583485260225E-17, 7.649999999999999467 ) ) ;
#17340 = AXIS2_PLACEMENT_3D ( 'NONE', #5914, #13213, #8957 ) ;
#17341 = CARTESIAN_POINT ( 'NONE',  ( 0.5291502622129179434, -6.480221748870319920E-17, 7.700000000000000178 ) ) ;
#17342 = CARTESIAN_POINT ( 'NONE',  ( 0.03895741673415010348, -1.870388906648449812, 2.647347042895590086 ) ) ;
#17343 = LINE ( 'NONE', #4568, #18238 ) ;
#17344 = CARTESIAN_POINT ( 'NONE',  ( 1.000000000000000000, 6.799999999999999822, 7.700000000000000178 ) ) ;
#17345 = VERTEX_POINT ( 'NONE', #4018 ) ;
#17346 = VECTOR ( 'NONE', #8171, 1000.000000000000000 ) ;
#17347 = VECTOR ( 'NONE', #3269, 1000.000000000000000 ) ;
#17348 = VECTOR ( 'NONE', #5586, 1000.000000000000000 ) ;
#17349 = LINE ( 'NONE', #10228, #8825 ) ;
#17350 = CARTESIAN_POINT ( 'NONE',  ( -2.105672170043390246, -1.637506023765568530, 3.084680091961149007 ) ) ;
#17351 = ORIENTED_EDGE ( 'NONE', *, *, #16602, .T. ) ;
#17352 = CARTESIAN_POINT ( 'NONE',  ( 2.102728310581320148, -4.241953435693879726, 5.757014351541050345 ) ) ;
#17353 = PLANE ( 'NONE',  #16072 ) ;
#17354 = DIRECTION ( 'NONE',  ( 3.652293603810800245E-15, 1.332267629550185876E-15, -1.000000000000000000 ) ) ;
#17355 = CARTESIAN_POINT ( 'NONE',  ( 2.043308330018790198, -5.099788135593220417, 5.867646457774659652 ) ) ;
#17356 = ORIENTED_EDGE ( 'NONE', *, *, #3584, .T. ) ;
#17357 = AXIS2_PLACEMENT_3D ( 'NONE', #4117, #8301, #16899 ) ;
#17358 = AXIS2_PLACEMENT_3D ( 'NONE', #8217, #6830, #16994 ) ;
#17359 = ORIENTED_EDGE ( 'NONE', *, *, #5974, .T. ) ;
#17360 = CARTESIAN_POINT ( 'NONE',  ( -1.899999999999999911, 11.40000000000000036, 1.600000000000000089 ) ) ;
#17361 = DIRECTION ( 'NONE',  ( 0.000000000000000000, 0.000000000000000000, 1.000000000000000000 ) ) ;
#17362 = VERTEX_POINT ( 'NONE', #5703 ) ;
#17364 = AXIS2_PLACEMENT_3D ( 'NONE', #8294, #1250, #5223 ) ;
#17363 = CIRCLE ( 'NONE', #529, 0.2500000000000002776 ) ;
#17365 = DIRECTION ( 'NONE',  ( -1.000000000000000000, 6.161988852941170860E-64, 6.123233995736769734E-17 ) ) ;
#17366 = CARTESIAN_POINT ( 'NONE',  ( -1.788074174585561060, -1.982989471729918352, 2.738902236199820539 ) ) ;
#17367 = EDGE_CURVE ( 'NONE', #14845, #5973, #6900, .T. ) ;
#17368 = AXIS2_PLACEMENT_3D ( 'NONE', #13715, #16671, #2784 ) ;
#17369 = CARTESIAN_POINT ( 'NONE',  ( 1.149999999999999911, 9.299999999999998934, 7.700000000000000178 ) ) ;
#17370 = LINE ( 'NONE', #13039, #7327 ) ;
#17371 = EDGE_CURVE ( 'NONE', #5801, #7791, #15917, .T. ) ;
#17372 = CARTESIAN_POINT ( 'NONE',  ( -0.5570002967655939274, -2.708767285026830063, 6.986590552960220357 ) ) ;
#17373 = CIRCLE ( 'NONE', #17922, 0.1499999999999999667 ) ;
#17374 = CARTESIAN_POINT ( 'NONE',  ( 0.5803392541454069908, -5.011796459788059543, 2.403119802722879950 ) ) ;
#17375 = AXIS2_PLACEMENT_3D ( 'NONE', #10789, #12093, #16250 ) ;
#17376 = CARTESIAN_POINT ( 'NONE',  ( -1.351547610267091581, -1.517223705964159786, 6.983951126925262542 ) ) ;
#17377 = AXIS2_PLACEMENT_3D ( 'NONE', #29, #12883, #16954 ) ;
#17378 = DIRECTION ( 'NONE',  ( 0.000000000000000000, 0.000000000000000000, 1.000000000000000000 ) ) ;
#17379 = CARTESIAN_POINT ( 'NONE',  ( -1.458615186838411626, -5.103620102360555855, 3.259477383973569786 ) ) ;
#17380 = VECTOR ( 'NONE', #9884, 1000.000000000000000 ) ;
#17381 = CIRCLE ( 'NONE', #9421, 0.5999999999999998668 ) ;
#17382 = LINE ( 'NONE', #7407, #1483 ) ;
#17383 = ORIENTED_EDGE ( 'NONE', *, *, #16019, .T. ) ;
#17384 = CARTESIAN_POINT ( 'NONE',  ( -0.5500000000000000444, 0.5999999999999999778, 1.600000000000000089 ) ) ;
#17385 = ORIENTED_EDGE ( 'NONE', *, *, #9516, .F. ) ;
#17386 = LINE ( 'NONE', #4989, #2601 ) ;
#17387 = CARTESIAN_POINT ( 'NONE',  ( 1.889999999999999902, 7.900000000000000355, 0.5999999999999999778 ) ) ;
#17388 = VECTOR ( 'NONE', #5710, 1000.000000000000000 ) ;
#17389 = EDGE_CURVE ( 'NONE', #1389, #103, #11348, .T. ) ;
#17390 = VERTEX_POINT ( 'NONE', #4295 ) ;
#17391 = EDGE_CURVE ( 'NONE', #16897, #7970, #14778, .T. ) ;
#17392 = CARTESIAN_POINT ( 'NONE',  ( -2.237394498046660019, -3.263845327585780165, 5.429939413646380331 ) ) ;
#17393 = EDGE_CURVE ( 'NONE', #8415, #14738, #17534, .T. ) ;
#17394 = FILL_AREA_STYLE ('',( #11766 ) ) ;
#17395 = CARTESIAN_POINT ( 'NONE',  ( 2.293398556041700065, -5.364194915254239859, 4.171956209133470317 ) ) ;
#17396 = EDGE_CURVE ( 'NONE', #7108, #3985, #14878, .T. ) ;
#17397 = DIRECTION ( 'NONE',  ( 0.000000000000000000, 0.000000000000000000, 1.000000000000000000 ) ) ;
#17398 = CARTESIAN_POINT ( 'NONE',  ( -1.854177340199669954, -1.610376859117309989, 6.149404042554720284 ) ) ;
#17399 = CARTESIAN_POINT ( 'NONE',  ( 1.866416942370620058, -3.962493976234419790, 3.266391446483460026 ) ) ;
#17400 = CARTESIAN_POINT ( 'NONE',  ( 1.998374131852729940, -0.9350164987569505870, 4.229465546630494011 ) ) ;
#17401 = DIRECTION ( 'NONE',  ( -1.233581138472399909E-16, 1.000000000000000000, 6.167905692361979821E-17 ) ) ;
#17402 = LINE ( 'NONE', #16036, #1467 ) ;
#17403 = ORIENTED_EDGE ( 'NONE', *, *, #10723, .T. ) ;
#17404 = CARTESIAN_POINT ( 'NONE',  ( 1.754713504580569960, -0.3489406779661023417, 3.634325740584615883 ) ) ;
#17405 = CARTESIAN_POINT ( 'NONE',  ( -2.237394498046660019, -3.263845327585780165, 5.429939413646380331 ) ) ;
#17406 = ORIENTED_EDGE ( 'NONE', *, *, #16421, .F. ) ;
#17407 = VECTOR ( 'NONE', #7339, 1000.000000000000000 ) ;
#17408 = ORIENTED_EDGE ( 'NONE', *, *, #10281, .T. ) ;
#17409 = DIRECTION ( 'NONE',  ( 1.000000000000000000, 0.000000000000000000, 0.000000000000000000 ) ) ;
#17410 = ORIENTED_EDGE ( 'NONE', *, *, #1840, .F. ) ;
#17411 = CARTESIAN_POINT ( 'NONE',  ( 0.8429265834919228428, -3.523857375116919766, 2.502678798553440220 ) ) ;
#17412 = CARTESIAN_POINT ( 'NONE',  ( 0.7998959936908462964, -5.135381355932194580, 7.230419212249866945 ) ) ;
#17413 = ADVANCED_FACE ( 'NONE', ( #3567 ), #5148, .F. ) ;
#17414 = PRODUCT_DEFINITION_FORMATION_WITH_SPECIFIED_SOURCE ( 'ANY', '', #8021, .NOT_KNOWN. ) ;
#17415 = CARTESIAN_POINT ( 'NONE',  ( -1.399999999999999911, -5.500000000000000000, 5.100000000000000533 ) ) ;
#17416 = CARTESIAN_POINT ( 'NONE',  ( 2.253200202764420013, -0.3889830508474579895, 5.379408587037500133 ) ) ;
#17417 = VERTEX_POINT ( 'NONE', #9214 ) ;
#17418 = DIRECTION ( 'NONE',  ( -1.000000000000000000, 0.000000000000000000, 0.000000000000000000 ) ) ;
#17419 = AXIS2_PLACEMENT_3D ( 'NONE', #7574, #7491, #15833 ) ;
#17420 = CARTESIAN_POINT ( 'NONE',  ( 1.503314099254039471, -3.939205687946139900, 3.301805249039985402 ) ) ;
#17421 = CARTESIAN_POINT ( 'NONE',  ( 1.000000000000000000, -5.000000000000000000, 3.299999999999999822 ) ) ;
#17422 = CARTESIAN_POINT ( 'NONE',  ( -2.630358833876468960, -0.5313559322033900578, 4.347767980622416317 ) ) ;
#17423 = ORIENTED_EDGE ( 'NONE', *, *, #9028, .T. ) ;
#17424 = CARTESIAN_POINT ( 'NONE',  ( 0.07299321914061039640, -0.3014830508474579673, 2.350000000000000089 ) ) ;
#17425 = CARTESIAN_POINT ( 'NONE',  ( -0.3042893218813459977, 6.450000000000000178, 2.170710678118660031 ) ) ;
#17426 = ADVANCED_FACE ( 'NONE', ( #14976 ), #11915, .F. ) ;
#17427 = EDGE_LOOP ( 'NONE', ( #8920, #4025, #7856, #1812 ) ) ;
#17428 = CARTESIAN_POINT ( 'NONE',  ( 0.009451942938127287294, -0.3001947080680037461, 2.339951117924002233 ) ) ;
#17429 = DIRECTION ( 'NONE',  ( 1.054711873393900133E-14, 1.000000000000000000, 0.000000000000000000 ) ) ;
#17430 = EDGE_CURVE ( 'NONE', #9511, #7811, #11472, .T. ) ;
#17431 = DIRECTION ( 'NONE',  ( -4.157615153618229646E-15, 1.000000000000000000, 1.972152263052530214E-30 ) ) ;
#17432 = VECTOR ( 'NONE', #10337, 1000.000000000000000 ) ;
#17433 = CARTESIAN_POINT ( 'NONE',  ( -0.2938780505772099483, -3.706322805063249959, 2.062434951628528523 ) ) ;
#17434 = ADVANCED_FACE ( 'NONE', ( #7836 ), #903, .F. ) ;
#17435 = ORIENTED_EDGE ( 'NONE', *, *, #11852, .F. ) ;
#17436 = CARTESIAN_POINT ( 'NONE',  ( -0.4539185741479770386, -3.384127645387189798, 2.390735265170449875 ) ) ;
#17437 = CARTESIAN_POINT ( 'NONE',  ( 1.399999999999999911, -5.500000000000000000, 5.100000000000000533 ) ) ;
#17438 = CARTESIAN_POINT ( 'NONE',  ( 0.1749999999999999889, 6.799999999999999822, 0.5999999999999999778 ) ) ;
#17439 = CARTESIAN_POINT ( 'NONE',  ( -1.566607907718199577, -4.432100618360157007, 6.026891670824300107 ) ) ;
#17440 = CARTESIAN_POINT ( 'NONE',  ( -0.5921572875253809931, 3.050000000000000266, 1.600000000000000089 ) ) ;
#17441 = CARTESIAN_POINT ( 'NONE',  ( -1.909909196654771213, -1.567641158900710430, 3.946907241329710381 ) ) ;
#17442 = ORIENTED_EDGE ( 'NONE', *, *, #7481, .T. ) ;
#17443 = CIRCLE ( 'NONE', #5658, 0.04999999999999991257 ) ;
#17444 = CARTESIAN_POINT ( 'NONE',  ( 0.9724415447670879953, -0.7068739681193980662, 2.553509270169310064 ) ) ;
#17445 = CARTESIAN_POINT ( 'NONE',  ( -2.471388659209118543, -1.381334852594401363, 5.667135868497515716 ) ) ;
#17446 = VERTEX_POINT ( 'NONE', #6541 ) ;
#17447 = CARTESIAN_POINT ( 'NONE',  ( -2.334748642087669523, -4.940602084342530453, 4.403867486184871005 ) ) ;
#17448 = DIRECTION ( 'NONE',  ( 1.000000000000000000, 0.000000000000000000, 0.000000000000000000 ) ) ;
#17449 = DIRECTION ( 'NONE',  ( -1.000000000000000000, 0.000000000000000000, 0.000000000000000000 ) ) ;
#17450 = CARTESIAN_POINT ( 'NONE',  ( -1.378221871957430178, -5.179872881355930048, 6.607619368096279366 ) ) ;
#17451 = ORIENTED_EDGE ( 'NONE', *, *, #12740, .T. ) ;
#17452 = ORIENTED_EDGE ( 'NONE', *, *, #4599, .F. ) ;
#17453 = DIRECTION ( 'NONE',  ( -1.000000000000000000, 0.000000000000000000, 7.401486830834370362E-16 ) ) ;
#17454 = DIRECTION ( 'NONE',  ( 6.123233995736767268E-17, -1.000000000000000000, 0.000000000000000000 ) ) ;
#17455 = ORIENTED_EDGE ( 'NONE', *, *, #8639, .F. ) ;
#17456 = VECTOR ( 'NONE', #16124, 1000.000000000000000 ) ;
#17457 = CARTESIAN_POINT ( 'NONE',  ( 1.875000000000000000, 11.25000000000000000, 7.700000000000000178 ) ) ;
#17458 = CARTESIAN_POINT ( 'NONE',  ( -2.556942001999829905, -1.843259742000191048, 3.989253004641622358 ) ) ;
#17459 = LINE ( 'NONE', #14687, #7332 ) ;
#17460 = CARTESIAN_POINT ( 'NONE',  ( -1.899999999999999911, 0.5999999999999999778, 7.599999999999999645 ) ) ;
#17461 = CARTESIAN_POINT ( 'NONE',  ( 1.465095039565329937, -2.033406924666469884, 2.858195935359850282 ) ) ;
#17462 = CARTESIAN_POINT ( 'NONE',  ( 1.873832970144350130, -5.337500000000000355, 2.826167029855650270 ) ) ;
#17463 = EDGE_CURVE ( 'NONE', #10646, #5474, #12195, .T. ) ;
#17464 = CARTESIAN_POINT ( 'NONE',  ( 2.022685914314938938, -1.167899381639830203, 6.418096442297061444 ) ) ;
#17465 = CARTESIAN_POINT ( 'NONE',  ( -1.850000000000000089, 11.25000000000000000, 7.649999999999999467 ) ) ;
#17466 = CARTESIAN_POINT ( 'NONE',  ( 0.5889081234606849957, -0.4379237288135600092, 6.978529000034869867 ) ) ;
#17467 = DIRECTION ( 'NONE',  ( -1.000000000000000000, 1.850371707708589879E-16, 0.000000000000000000 ) ) ;
#17468 = ORIENTED_EDGE ( 'NONE', *, *, #3500, .F. ) ;
#17469 = DIRECTION ( 'NONE',  ( 1.480297366166879989E-16, 7.401486830834378990E-17, -1.000000000000000000 ) ) ;
#17470 = ORIENTED_EDGE ( 'NONE', *, *, #10395, .T. ) ;
#17471 = EDGE_CURVE ( 'NONE', #2611, #4443, #16169, .T. ) ;
#17472 = CARTESIAN_POINT ( 'NONE',  ( 2.500000000000000000, -3.214554059336160952E-17, 4.000000000000000000 ) ) ;
#17473 = DIRECTION ( 'NONE',  ( 1.000000000000000000, 0.000000000000000000, 1.168655815394900078E-16 ) ) ;
#17474 = ORIENTED_EDGE ( 'NONE', *, *, #16302, .T. ) ;
#17475 = CARTESIAN_POINT ( 'NONE',  ( -2.267872052190610166, -1.843259742000189938, 4.071110468860649867 ) ) ;
#17476 = DIRECTION ( 'NONE',  ( 1.000000000000000000, 1.283953296258166085E-32, -6.123233995736769734E-17 ) ) ;
#17477 = LINE ( 'NONE', #11941, #17625 ) ;
#17478 = CARTESIAN_POINT ( 'NONE',  ( -2.350000000000000089, -6.000000000000000000, 6.400000000000000355 ) ) ;
#17479 = CARTESIAN_POINT ( 'NONE',  ( 2.351212046067109984, -0.9815930753335269099, 4.597298481426010497 ) ) ;
#17480 = CARTESIAN_POINT ( 'NONE',  ( -1.465095039565370127, -3.566593075333519991, 2.858195935359880480 ) ) ;
#17481 = CARTESIAN_POINT ( 'NONE',  ( 1.785776242921180756, -1.121322805063259542, 5.712869711683790541 ) ) ;
#17482 = EDGE_CURVE ( 'NONE', #356, #8350, #797, .T. ) ;
#17483 = CARTESIAN_POINT ( 'NONE',  ( 0.1749999999999999889, 7.500000000000000000, 1.600000000000000089 ) ) ;
#17484 = PRODUCT_RELATED_PRODUCT_CATEGORY ( 'part', '', ( #4881 ) ) ;
#17485 = FACE_OUTER_BOUND ( 'NONE', #3995, .T. ) ;
#17486 = EDGE_LOOP ( 'NONE', ( #7982, #12539, #1304, #18011 ) ) ;
#17487 = EDGE_CURVE ( 'NONE', #4854, #13116, #9121, .T. ) ;
#17488 = CARTESIAN_POINT ( 'NONE',  ( 0.9222751404130974384, -0.3222457627118649470, 2.865854510788131027 ) ) ;
#17489 = CARTESIAN_POINT ( 'NONE',  ( 0.1824815401350060040, -4.498124606865050445, 7.046368721022729709 ) ) ;
#17490 = ORIENTED_EDGE ( 'NONE', *, *, #11291, .F. ) ;
#17491 = ADVANCED_FACE ( 'NONE', ( #9308 ), #12106, .T. ) ;
#17492 = VERTEX_POINT ( 'NONE', #2287 ) ;
#17493 = EDGE_CURVE ( 'NONE', #9105, #16183, #16797, .T. ) ;
#17494 = CARTESIAN_POINT ( 'NONE',  ( 1.800000000000000044, 12.00000000000000000, 1.600000000000000089 ) ) ;
#17495 = ORIENTED_EDGE ( 'NONE', *, *, #8391, .T. ) ;
#17496 = CARTESIAN_POINT ( 'NONE',  ( -1.704669856830349772, -4.796950468210010143, 3.080704711052660194 ) ) ;
#17497 = CONTEXT_DEPENDENT_SHAPE_REPRESENTATION ( #11578, #12157 ) ;
#17498 = CARTESIAN_POINT ( 'NONE',  ( -1.973760952634090238, -5.559957627118640389, 2.925986839873730982 ) ) ;
#17499 = LINE ( 'NONE', #15968, #17347 ) ;
#17500 = CARTESIAN_POINT ( 'NONE',  ( 0.1565249325564390115, -0.4468220338983060480, 7.048192310558509810 ) ) ;
#17501 = VERTEX_POINT ( 'NONE', #3754 ) ;
#17502 = LINE ( 'NONE', #11797, #7577 ) ;
#17503 = FACE_OUTER_BOUND ( 'NONE', #11097, .T. ) ;
#17504 = CARTESIAN_POINT ( 'NONE',  ( 0.7128755192781456307, -3.822764246504686270, 2.774718115017441367 ) ) ;
#17505 = CARTESIAN_POINT ( 'NONE',  ( 2.354888465609351389, -0.09788135593220394226, 5.923664702843856489 ) ) ;
#17506 = ORIENTED_EDGE ( 'NONE', *, *, #11229, .F. ) ;
#17507 = FACE_OUTER_BOUND ( 'NONE', #10947, .T. ) ;
#17508 = ORIENTED_EDGE ( 'NONE', *, *, #7588, .F. ) ;
#17509 = EDGE_CURVE ( 'NONE', #5262, #9388, #9416, .T. ) ;
#17510 = CARTESIAN_POINT ( 'NONE',  ( 2.638803263991410741, -0.3800847457627119508, 4.982085668537405532 ) ) ;
#17511 = ORIENTED_EDGE ( 'NONE', *, *, #7007, .T. ) ;
#17512 = CARTESIAN_POINT ( 'NONE',  ( 1.112838723655040107, -5.426483050847459744, 6.773667561836210105 ) ) ;
#17513 = CARTESIAN_POINT ( 'NONE',  ( -2.234315482767909700, -0.2402542372881359967, 3.960850823455329905 ) ) ;
#17514 = CARTESIAN_POINT ( 'NONE',  ( -0.7756407636288503715, -4.591277760018214416, 7.238010066725332869 ) ) ;
#17515 = ORIENTED_EDGE ( 'NONE', *, *, #15014, .F. ) ;
#17516 = CARTESIAN_POINT ( 'NONE',  ( -1.444955263746759977, -3.267686203945750378, 2.842353646881510265 ) ) ;
#17517 = FACE_OUTER_BOUND ( 'NONE', #6309, .T. ) ;
#17518 = LINE ( 'NONE', #7217, #9244 ) ;
#17519 = CARTESIAN_POINT ( 'NONE',  ( -1.404946080800599351, -3.244397915657463827, 3.202993536195951840 ) ) ;
#17520 = LINE ( 'NONE', #14406, #8555 ) ;
#17521 = CARTESIAN_POINT ( 'NONE',  ( -1.224086244040909488, -1.241605122864670285, 6.348185277745776567 ) ) ;
#17522 = ORIENTED_EDGE ( 'NONE', *, *, #2064, .T. ) ;
#17523 = DIRECTION ( 'NONE',  ( 1.110223024625159992E-16, 0.000000000000000000, -1.000000000000000000 ) ) ;
#17524 = ADVANCED_FACE ( 'NONE', ( #8039 ), #618, .F. ) ;
#17525 = CARTESIAN_POINT ( 'NONE',  ( 1.850000000000000089, 0.7500000000000000000, 8.300000000000000711 ) ) ;
#17526 = ORIENTED_EDGE ( 'NONE', *, *, #9832, .F. ) ;
#17527 = CARTESIAN_POINT ( 'NONE',  ( 1.800000000000000044, 11.29999999999999893, 7.649999999999999467 ) ) ;
#17528 = DIRECTION ( 'NONE',  ( -1.000000000000000000, 0.000000000000000000, 0.000000000000000000 ) ) ;
#17529 = DIRECTION ( 'NONE',  ( 0.000000000000000000, 0.000000000000000000, 1.000000000000000000 ) ) ;
#17530 = CARTESIAN_POINT ( 'NONE',  ( -0.6493550500446439999, -5.286652542372879182, 2.437955526623099889 ) ) ;
#17531 = ORIENTED_EDGE ( 'NONE', *, *, #17253, .F. ) ;
#17532 = VERTEX_POINT ( 'NONE', #12284 ) ;
#17533 = FACE_OUTER_BOUND ( 'NONE', #17667, .T. ) ;
#17534 = LINE ( 'NONE', #6339, #6741 ) ;
#17535 = CARTESIAN_POINT ( 'NONE',  ( 1.250000000000000000, 7.799999999999999822, 7.599999999999999645 ) ) ;
#17536 = ORIENTED_EDGE ( 'NONE', *, *, #6417, .F. ) ;
#17537 = LINE ( 'NONE', #709, #559 ) ;
#17538 = CARTESIAN_POINT ( 'NONE',  ( -0.8400312909772689185, -3.030962444702889780, 7.217431453521816920 ) ) ;
#17539 = LINE ( 'NONE', #6346, #2000 ) ;
#17540 = CARTESIAN_POINT ( 'NONE',  ( 2.500000000000000000, 7.299999999999999822, 0.6099999999999999867 ) ) ;
#17541 = CARTESIAN_POINT ( 'NONE',  ( 2.308170020371300257, -3.873181699441239800, 5.159452766389609479 ) ) ;
#17542 = CARTESIAN_POINT ( 'NONE',  ( 0.009452110982655418520, -5.000192044704539818, 2.350000000000000089 ) ) ;
#17544 = ORIENTED_EDGE ( 'NONE', *, *, #1088, .T. ) ;
#17543 = CARTESIAN_POINT ( 'NONE',  ( -2.644456467089570939, -1.796683165423619055, 4.476474416072687035 ) ) ;
#17545 = VECTOR ( 'NONE', #10750, 1000.000000000000000 ) ;
#17546 = DIRECTION ( 'NONE',  ( 0.000000000000000000, 0.000000000000000000, 1.000000000000000000 ) ) ;
#17547 = LINE ( 'NONE', #10917, #13553 ) ;
#17548 = CARTESIAN_POINT ( 'NONE',  ( -1.800000000000000044, 0.5999999999999999778, 6.599999999999999645 ) ) ;
#17549 = FACE_OUTER_BOUND ( 'NONE', #11253, .T. ) ;
#17550 = ORIENTED_EDGE ( 'NONE', *, *, #3364, .F. ) ;
#17551 = DIRECTION ( 'NONE',  ( 1.000000000000000000, 0.000000000000000000, -2.467162276944790449E-16 ) ) ;
#17552 = EDGE_LOOP ( 'NONE', ( #14870, #4166, #7646, #190 ) ) ;
#17553 = DIRECTION ( 'NONE',  ( -1.000000000000000000, 2.220446049250315053E-16, 6.049014748177260544E-16 ) ) ;
#17554 = CARTESIAN_POINT ( 'NONE',  ( -1.300000000000000044, 1.592040838891560081E-16, 7.599999999999999645 ) ) ;
#17555 = ORIENTED_EDGE ( 'NONE', *, *, #4151, .F. ) ;
#17556 = CARTESIAN_POINT ( 'NONE',  ( -1.507201387235980183, -3.124115597856050197, 6.507509243627219497 ) ) ;
#17557 = CARTESIAN_POINT ( 'NONE',  ( 0.7093417302541469294, -5.435381355932199732, 6.943956659919690466 ) ) ;
#17558 = CARTESIAN_POINT ( 'NONE',  ( 1.000000000000000000, -5.599999999999999645, 3.673738709727309981 ) ) ;
#17559 = VECTOR ( 'NONE', #7140, 1000.000000000000000 ) ;
#17560 = CARTESIAN_POINT ( 'NONE',  ( 1.115198193348289957, -1.261052534792989954, 6.772457159276550342 ) ) ;
#17561 = CARTESIAN_POINT ( 'NONE',  ( 1.397172971746949877, -3.892629111369559691, 2.806153814454899642 ) ) ;
#17562 = CARTESIAN_POINT ( 'NONE',  ( 1.138568046961060176, -1.237764246504700072, 6.408380708468512488 ) ) ;
#17563 = DIRECTION ( 'NONE',  ( 0.000000000000000000, 0.000000000000000000, -1.000000000000000000 ) ) ;
#17564 = DIRECTION ( 'NONE',  ( 1.000000000000000000, -2.220446049250309876E-16, 0.000000000000000000 ) ) ;
#17565 = ORIENTED_EDGE ( 'NONE', *, *, #13426, .T. ) ;
#17566 = CARTESIAN_POINT ( 'NONE',  ( 0.06367493584606445656, -0.3014830508474583004, 2.649999999999998579 ) ) ;
#17567 = CARTESIAN_POINT ( 'NONE',  ( 2.192143888961729736, -4.218665147405599392, 5.556300681753580051 ) ) ;
#17568 = EDGE_LOOP ( 'NONE', ( #10677, #8399, #12990, #6028 ) ) ;
#17569 = ORIENTED_EDGE ( 'NONE', *, *, #3094, .T. ) ;
#17570 = DIRECTION ( 'NONE',  ( 0.000000000000000000, 0.000000000000000000, -1.000000000000000000 ) ) ;
#17571 = ORIENTED_EDGE ( 'NONE', *, *, #1843, .F. ) ;
#17572 = CARTESIAN_POINT ( 'NONE',  ( -2.351212046067109984, -4.618406924666470736, 4.597298481426070893 ) ) ;
#17573 = CARTESIAN_POINT ( 'NONE',  ( 2.332582362116870200, -5.068644067796610031, 4.387643303570810005 ) ) ;
#17574 = CARTESIAN_POINT ( 'NONE',  ( 1.899999999999999911, 11.40000000000000036, 7.550000000000000711 ) ) ;
#17575 = CARTESIAN_POINT ( 'NONE',  ( 1.000896394980339998, -0.4290254237288140260, 6.829956240957369751 ) ) ;
#17576 = VERTEX_POINT ( 'NONE', #17905 ) ;
#17577 = APPLICATION_CONTEXT ( 'automotive_design' ) ;
#17578 = EDGE_CURVE ( 'NONE', #651, #17998, #9594, .T. ) ;
#17579 = EDGE_CURVE ( 'NONE', #12508, #4345, #4956, .T. ) ;
#17580 = CARTESIAN_POINT ( 'NONE',  ( -0.4114611322411360628, -4.567989471729919870, 6.711368086473216366 ) ) ;
#17581 = EDGE_CURVE ( 'NONE', #17808, #4810, #10990, .T. ) ;
#17582 = CARTESIAN_POINT ( 'NONE',  ( -2.508228811380011081, -0.5091101694915260989, 5.566973598334550744 ) ) ;
#17583 = ORIENTED_EDGE ( 'NONE', *, *, #17471, .T. ) ;
#17584 = CARTESIAN_POINT ( 'NONE',  ( 0.8570167067220200163, -0.3177966101694920664, 2.508190348879349774 ) ) ;
#17585 = CARTESIAN_POINT ( 'NONE',  ( 1.250000000000000000, 3.500000000000000000, 6.100000000000000533 ) ) ;
#17586 = CARTESIAN_POINT ( 'NONE',  ( -0.07064654565474801085, -0.4512711864406789841, 7.352897294663512717 ) ) ;
#17587 = ORIENTED_EDGE ( 'NONE', *, *, #2379, .F. ) ;
#17588 = CARTESIAN_POINT ( 'NONE',  ( -3.408368997776849933E-15, -5.599999999999999645, 2.350000000000000089 ) ) ;
#17589 = AXIS2_PLACEMENT_3D ( 'NONE', #8026, #7571, #11647 ) ;
#17590 = CARTESIAN_POINT ( 'NONE',  ( -1.219286470748950135, -1.218316834576380403, 6.712979431025679844 ) ) ;
#17591 = CARTESIAN_POINT ( 'NONE',  ( -0.3897427956305680175, -0.2909039927201511055, 2.676097687607990938 ) ) ;
#17592 = CARTESIAN_POINT ( 'NONE',  ( 1.769056124370469885, -3.915917399657852904, 2.721729512470748791 ) ) ;
#17593 = VERTEX_POINT ( 'NONE', #7002 ) ;
#17594 = ADVANCED_FACE ( 'NONE', ( #18275 ), #12380, .T. ) ;
#17595 = CARTESIAN_POINT ( 'NONE',  ( -0.009452110982656853136, -5.299807955295470663, 2.649999999999998579 ) ) ;
#17596 = CARTESIAN_POINT ( 'NONE',  ( 2.199335452462550133, -3.733451969711520491, 3.862342996790889771 ) ) ;
#17597 = ADVANCED_FACE ( 'NONE', ( #5433 ), #8310, .T. ) ;
#17598 = CARTESIAN_POINT ( 'NONE',  ( 1.500000000000000000, -5.599999999999999645, 2.299999999999999822 ) ) ;
#17599 = DIRECTION ( 'NONE',  ( 0.000000000000000000, -1.000000000000000000, 6.123233995736769734E-17 ) ) ;
#17600 = EDGE_CURVE ( 'NONE', #15355, #4874, #11197, .T. ) ;
#17601 = CARTESIAN_POINT ( 'NONE',  ( 1.079900583135640302, -3.570433951693503527, 2.953942563037689428 ) ) ;
#17602 = CIRCLE ( 'NONE', #3146, 0.04999999999999969746 ) ;
#17603 = CARTESIAN_POINT ( 'NONE',  ( 0.4000000000000000222, -1.399999999999999911, 5.100000000000000533 ) ) ;
#17604 = DIRECTION ( 'NONE',  ( -2.055968564120659776E-16, -1.000000000000000000, 0.000000000000000000 ) ) ;
#17605 = VECTOR ( 'NONE', #1333, 1000.000000000000000 ) ;
#17606 = CARTESIAN_POINT ( 'NONE',  ( -1.627161714697918704, -1.637506023765568530, 3.448102801005849649 ) ) ;
#17607 = ORIENTED_EDGE ( 'NONE', *, *, #6435, .T. ) ;
#17608 = CARTESIAN_POINT ( 'NONE',  ( 0.1749999999999999889, 7.900000000000000355, 0.5999999999999999778 ) ) ;
#17609 = CARTESIAN_POINT ( 'NONE',  ( 0.000000000000000000, 0.000000000000000000, 7.599999999999999645 ) ) ;
#17610 = CARTESIAN_POINT ( 'NONE',  ( -1.155768864438580179, -1.195028546288090743, 7.088998121597467339 ) ) ;
#17611 = ORIENTED_EDGE ( 'NONE', *, *, #13906, .T. ) ;
#17612 = CARTESIAN_POINT ( 'NONE',  ( 1.889999999999999902, 4.700000000000000178, 0.5999999999999999778 ) ) ;
#17613 = LINE ( 'NONE', #11042, #17225 ) ;
#17614 = VECTOR ( 'NONE', #1748, 1000.000000000000000 ) ;
#17615 = CARTESIAN_POINT ( 'NONE',  ( -1.550000000000000044, -5.599999999999999645, 6.100000000000000533 ) ) ;
#17616 = CARTESIAN_POINT ( 'NONE',  ( 1.880631435828169939, -5.055296610169490279, 3.876649216148224220 ) ) ;
#17617 = ORIENTED_EDGE ( 'NONE', *, *, #17863, .F. ) ;
#17618 = ORIENTED_EDGE ( 'NONE', *, *, #12249, .F. ) ;
#17619 = CARTESIAN_POINT ( 'NONE',  ( 0.6500000000000000222, 6.450000000000000178, 3.200000000000000178 ) ) ;
#17620 = DIRECTION ( 'NONE',  ( 0.000000000000000000, 0.000000000000000000, -1.000000000000000000 ) ) ;
#17621 = DIRECTION ( 'NONE',  ( 0.000000000000000000, -1.000000000000000000, 0.000000000000000000 ) ) ;
#17622 = ORIENTED_EDGE ( 'NONE', *, *, #9762, .F. ) ;
#17623 = AXIS2_PLACEMENT_3D ( 'NONE', #9719, #7220, #12584 ) ;
#17624 = CARTESIAN_POINT ( 'NONE',  ( -1.846259792136611066, -5.546610169491530407, 3.802221692020929744 ) ) ;
#17625 = VECTOR ( 'NONE', #10106, 1000.000000000000000 ) ;
#17626 = CARTESIAN_POINT ( 'NONE',  ( -0.1366863161730529075, -2.662190708450249854, 7.350364228549148393 ) ) ;
#17627 = CARTESIAN_POINT ( 'NONE',  ( 1.428323476796560465, -2.309025507765959606, 2.463260019887501429 ) ) ;
#17628 = EDGE_CURVE ( 'NONE', #2153, #8790, #9509, .T. ) ;
#17629 = CARTESIAN_POINT ( 'NONE',  ( 1.800000000000000044, 11.40000000000000036, 6.599999999999999645 ) ) ;
#17630 = LINE ( 'NONE', #7950, #6375 ) ;
#17631 = AXIS2_PLACEMENT_3D ( 'NONE', #12159, #16681, #1135 ) ;
#17632 = CARTESIAN_POINT ( 'NONE',  ( 2.267872052190590182, -3.756740257999799937, 4.071110468860600129 ) ) ;
#17633 = VECTOR ( 'NONE', #1772, 1000.000000000000000 ) ;
#17634 = LINE ( 'NONE', #3580, #9971 ) ;
#17635 = CARTESIAN_POINT ( 'NONE',  ( 2.500000000000000000, 10.00000000000000000, 1.600000000000000089 ) ) ;
#17637 = ORIENTED_EDGE ( 'NONE', *, *, #4267, .F. ) ;
#17636 = CARTESIAN_POINT ( 'NONE',  ( -1.071153154657450202, -3.054250732991181216, 7.128115444592631356 ) ) ;
#17638 = AXIS2_PLACEMENT_3D ( 'NONE', #9011, #12929, #257 ) ;
#17639 = DIRECTION ( 'NONE',  ( 0.000000000000000000, 0.000000000000000000, 1.000000000000000000 ) ) ;
#17640 = CIRCLE ( 'NONE', #4064, 0.1000000000000000472 ) ;
#17641 = CARTESIAN_POINT ( 'NONE',  ( 1.850000000000000089, -6.000000000000000000, 6.899999999999999467 ) ) ;
#17642 = CARTESIAN_POINT ( 'NONE',  ( 2.046174187462399985, -1.121322805063259986, 5.862719605943959245 ) ) ;
#17643 = DIRECTION ( 'NONE',  ( -9.796085511398438540E-17, -8.106125845929150651E-31, -1.000000000000000000 ) ) ;
#17644 = CARTESIAN_POINT ( 'NONE',  ( 2.321479326063749404, -5.350847457627126325, 3.414080590619961608 ) ) ;
#17645 = EDGE_LOOP ( 'NONE', ( #4920, #10558, #4076, #6748, #16323, #3627 ) ) ;
#17646 = EDGE_CURVE ( 'NONE', #4096, #11111, #8209, .T. ) ;
#17647 = LINE ( 'NONE', #3593, #13734 ) ;
#17648 = ORIENTED_EDGE ( 'NONE', *, *, #4872, .F. ) ;
#17649 = DIRECTION ( 'NONE',  ( -1.000000000000000000, 0.000000000000000000, 0.000000000000000000 ) ) ;
#17650 = LINE ( 'NONE', #17554, #15654 ) ;
#17651 = VECTOR ( 'NONE', #3091, 1000.000000000000000 ) ;
#17652 = VERTEX_POINT ( 'NONE', #16906 ) ;
#17653 = EDGE_CURVE ( 'NONE', #389, #13169, #11072, .T. ) ;
#17654 = VERTEX_POINT ( 'NONE', #12468 ) ;
#17655 = CARTESIAN_POINT ( 'NONE',  ( -1.332058588847369940, -3.100827309567760537, 6.640197310420220767 ) ) ;
#17656 = EDGE_CURVE ( 'NONE', #11991, #14398, #16716, .T. ) ;
#17657 = AXIS2_PLACEMENT_3D ( 'NONE', #18077, #5425, #1539 ) ;
#17658 = DIRECTION ( 'NONE',  ( 1.000000000000000000, 0.000000000000000000, -7.401486830834380223E-16 ) ) ;
#17659 = DIRECTION ( 'NONE',  ( 0.000000000000000000, 0.000000000000000000, -1.000000000000000000 ) ) ;
#17660 = LINE ( 'NONE', #16581, #469 ) ;
#17661 = CARTESIAN_POINT ( 'NONE',  ( -1.881914957835490121, -1.936412895153350133, 3.286797332666350435 ) ) ;
#17662 = CARTESIAN_POINT ( 'NONE',  ( 2.343457872958619959, -4.148800282540729967, 4.916681529328559286 ) ) ;
#17663 = VECTOR ( 'NONE', #289, 1000.000000000000000 ) ;
#17664 = CARTESIAN_POINT ( 'NONE',  ( -1.642659730162759901, -1.936412895153350133, 3.468508687188699646 ) ) ;
#17665 = DIRECTION ( 'NONE',  ( -1.556829778943089964E-16, 0.000000000000000000, 1.000000000000000000 ) ) ;
#17666 = DIRECTION ( 'NONE',  ( 0.000000000000000000, -1.000000000000000000, 0.000000000000000000 ) ) ;
#17667 = EDGE_LOOP ( 'NONE', ( #16356, #2659, #16191, #3489, #3189, #632, #4321, #5615 ) ) ;
#17668 = VECTOR ( 'NONE', #13651, 1000.000000000000000 ) ;
#17669 = CARTESIAN_POINT ( 'NONE',  ( 1.550000000000000044, -6.000000000000000000, 6.100000000000000533 ) ) ;
#17670 = CARTESIAN_POINT ( 'NONE',  ( -2.062913653388399826, -3.217268751009200400, 5.832754583370829415 ) ) ;
#17671 = ORIENTED_EDGE ( 'NONE', *, *, #18172, .F. ) ;
#17672 = VERTEX_POINT ( 'NONE', #1349 ) ;
#17673 = DIRECTION ( 'NONE',  ( 1.110223024625160090E-15, 1.000000000000000000, 0.000000000000000000 ) ) ;
#17674 = ORIENTED_EDGE ( 'NONE', *, *, #17153, .F. ) ;
#17675 = LINE ( 'NONE', #5015, #14231 ) ;
#17676 = AXIS2_PLACEMENT_3D ( 'NONE', #13987, #5301, #1305 ) ;
#17677 = APPLICATION_PROTOCOL_DEFINITION ( 'draft international standard', 'automotive_design', 1998, #17577 ) ;
#17678 = CARTESIAN_POINT ( 'NONE',  ( -1.707817112497179934, -5.188771186440679806, 6.319218296629480314 ) ) ;
#17679 = VECTOR ( 'NONE', #12801, 1000.000000000000000 ) ;
#17680 = DIRECTION ( 'NONE',  ( -5.551115123125880521E-15, 1.000000000000000000, 6.055990775824630636E-30 ) ) ;
#17681 = AXIS2_PLACEMENT_3D ( 'NONE', #11191, #16836, #4146 ) ;
#17682 = DIRECTION ( 'NONE',  ( 1.224646799147351975E-16, -1.000000000000000000, -6.123233995736789455E-17 ) ) ;
#17683 = CARTESIAN_POINT ( 'NONE',  ( -0.9516466452860307124, -4.637854336594775084, 6.519140045500596337 ) ) ;
#17684 = EDGE_CURVE ( 'NONE', #16414, #5991, #6758, .T. ) ;
#17685 = CARTESIAN_POINT ( 'NONE',  ( -0.5609751937345790473, -0.4601694915254239682, 7.293870047334757523 ) ) ;
#17686 = ORIENTED_EDGE ( 'NONE', *, *, #111, .T. ) ;
#17687 = CARTESIAN_POINT ( 'NONE',  ( 2.203023580853990193, -0.3578389830508479919, 3.872235369154280349 ) ) ;
#17688 = AXIS2_PLACEMENT_3D ( 'NONE', #6612, #9103, #688 ) ;
#17689 = CARTESIAN_POINT ( 'NONE',  ( -1.134881315981510541, -0.4779661016949154906, 6.410767520434657918 ) ) ;
#17690 = CARTESIAN_POINT ( 'NONE',  ( -2.171642826483958899, -0.1957627118644069686, 6.225392547715731695 ) ) ;
#17691 = ORIENTED_EDGE ( 'NONE', *, *, #1266, .F. ) ;
#17692 = CARTESIAN_POINT ( 'NONE',  ( 7.771561172376099727E-16, 5.131370849898479136, 5.100000000000000533 ) ) ;
#17693 = CYLINDRICAL_SURFACE ( 'NONE', #7954, 0.4000000000000000222 ) ;
#17694 = CARTESIAN_POINT ( 'NONE',  ( 2.484260633728970546, -0.3578389830508479363, 3.766563288620793593 ) ) ;
#17695 = CARTESIAN_POINT ( 'NONE',  ( 2.135041058613649234, -0.7991276453871951624, 5.690123914223770285 ) ) ;
#17696 = EDGE_CURVE ( 'NONE', #17047, #2205, #1175, .T. ) ;
#17697 = CARTESIAN_POINT ( 'NONE',  ( 2.332582362116870200, -5.368644067796609853, 4.387643303570810005 ) ) ;
#17698 = CARTESIAN_POINT ( 'NONE',  ( -1.940935473245981147, -5.095857339597785973, 2.893832807158200016 ) ) ;
#17699 = EDGE_LOOP ( 'NONE', ( #2637, #2554, #3705, #17406 ) ) ;
#17700 = CARTESIAN_POINT ( 'NONE',  ( 1.399999999999999911, -5.000000000000000000, 3.299999999999999822 ) ) ;
#17701 = AXIS2_PLACEMENT_3D ( 'NONE', #1318, #6965, #2997 ) ;
#17702 = CARTESIAN_POINT ( 'NONE',  ( -1.962536940652960027, -2.895073591333140239, 5.998920491814800471 ) ) ;
#17703 = CARTESIAN_POINT ( 'NONE',  ( 2.107551805806971323, -4.288530012270460823, 6.312866726931170902 ) ) ;
#17704 = CARTESIAN_POINT ( 'NONE',  ( 1.750000000000000000, 11.40000000000000036, 7.700000000000000178 ) ) ;
#17705 = DIRECTION ( 'NONE',  ( 1.059965646700398694E-16, 0.6823182503600109250, 0.7310552682428693716 ) ) ;
#17706 = CARTESIAN_POINT ( 'NONE',  ( 1.750352751699790987, -3.686875393134939394, 3.627075451280439733 ) ) ;
#17707 = DIRECTION ( 'NONE',  ( -1.224646799147350002E-16, 1.000000000000000000, 6.123233995736769734E-17 ) ) ;
#17708 = CARTESIAN_POINT ( 'NONE',  ( 0.03000000000000110217, 11.40000000000000036, 7.649999999999999467 ) ) ;
#17709 = CARTESIAN_POINT ( 'NONE',  ( 0.4194839839381755975, -1.916965483225031130, 2.690289814463930895 ) ) ;
#17710 = VERTEX_POINT ( 'NONE', #18086 ) ;
#17711 = CARTESIAN_POINT ( 'NONE',  ( 1.800000000000000044, 0.5999999999999999778, 6.599999999999999645 ) ) ;
#17712 = CARTESIAN_POINT ( 'NONE',  ( 2.500000000000000000, 9.199999999999999289, 0.5999999999999999778 ) ) ;
#17713 = ADVANCED_FACE ( 'NONE', ( #9681 ), #14798, .T. ) ;
#17714 = CARTESIAN_POINT ( 'NONE',  ( 0.4904671284965613776, -0.6606104644819267291, 2.692290850878278796 ) ) ;
#17715 = CARTESIAN_POINT ( 'NONE',  ( 0.3578984759184136166, -2.615614131873680748, 7.329643012642057087 ) ) ;
#17716 = ORIENTED_EDGE ( 'NONE', *, *, #1720, .T. ) ;
#17717 = VECTOR ( 'NONE', #3960, 1000.000000000000000 ) ;
#17718 = DIRECTION ( 'NONE',  ( 0.000000000000000000, 0.000000000000000000, 1.000000000000000000 ) ) ;
#17719 = CARTESIAN_POINT ( 'NONE',  ( 1.928817277882869829, -1.144611093351550091, 6.048484184565929844 ) ) ;
#17720 = FACE_OUTER_BOUND ( 'NONE', #8788, .T. ) ;
#17721 = CARTESIAN_POINT ( 'NONE',  ( 1.112838723655040107, -5.126483050847459921, 6.773667561836210105 ) ) ;
#17722 = EDGE_LOOP ( 'NONE', ( #42, #3963, #3279, #4123 ) ) ;
#17723 = EDGE_CURVE ( 'NONE', #16395, #9909, #11806, .T. ) ;
#17724 = ORIENTED_EDGE ( 'NONE', *, *, #13543, .T. ) ;
#17725 = CYLINDRICAL_SURFACE ( 'NONE', #8892, 0.6000000000000000888 ) ;
#17726 = EDGE_CURVE ( 'NONE', #3220, #10706, #7627, .T. ) ;
#17727 = CARTESIAN_POINT ( 'NONE',  ( 1.399999999999999911, -5.000000000000000000, 3.299999999999999822 ) ) ;
#17728 = DIRECTION ( 'NONE',  ( -2.220446049250309876E-16, 0.000000000000000000, 1.000000000000000000 ) ) ;
#17729 = VERTEX_POINT ( 'NONE', #6232 ) ;
#17730 = CARTESIAN_POINT ( 'NONE',  ( -1.754713504580578842, -5.551059322033894183, 3.634325740584633646 ) ) ;
#17731 = ADVANCED_FACE ( 'NONE', ( #769 ), #3357, .T. ) ;
#17732 = CARTESIAN_POINT ( 'NONE',  ( -0.9880847989278745969, -3.337551068810613142, 2.236912075639700515 ) ) ;
#17733 = CARTESIAN_POINT ( 'NONE',  ( 0.9930264841371563289, -0.4076464065212259125, 2.562902636367420772 ) ) ;
#17734 = DIRECTION ( 'NONE',  ( -1.340940200278649995E-16, 1.000000000000000000, 0.000000000000000000 ) ) ;
#17735 = LINE ( 'NONE', #5064, #12350 ) ;
#17736 = VECTOR ( 'NONE', #4477, 1000.000000000000000 ) ;
#17737 = CARTESIAN_POINT ( 'NONE',  ( 1.381042549632460092, -4.059488005747549977, 6.605640880016110827 ) ) ;
#17738 = CARTESIAN_POINT ( 'NONE',  ( -2.350000000000000089, -5.599999999999999645, 2.799999999999999822 ) ) ;
#17739 = CARTESIAN_POINT ( 'NONE',  ( -0.03000000000000000236, 11.40000000000000036, -2.869354249208270301E-17 ) ) ;
#17740 = CARTESIAN_POINT ( 'NONE',  ( -0.4722227023514615762, -2.122719201459649874, 2.088464165977090836 ) ) ;
#17741 = ADVANCED_FACE ( 'NONE', ( #6402 ), #17693, .F. ) ;
#17742 = LINE ( 'NONE', #10632, #4978 ) ;
#17743 = DIRECTION ( 'NONE',  ( 6.938893903907229610E-17, 0.000000000000000000, 1.000000000000000000 ) ) ;
#17744 = CARTESIAN_POINT ( 'NONE',  ( 1.444955263746720009, -2.332313796054249710, 2.842353646881480511 ) ) ;
#17745 = CARTESIAN_POINT ( 'NONE',  ( -2.350067830300900162, -0.5224576271186440746, 4.825253242917699303 ) ) ;
#17746 = CARTESIAN_POINT ( 'NONE',  ( -0.4000000000000000222, 2.399999999999999911, 5.100000000000000533 ) ) ;
#17747 = ORIENTED_EDGE ( 'NONE', *, *, #11970, .T. ) ;
#17748 = PRODUCT ( 'Actuator Return Helical Spring', 'Actuator Return Helical Spring', '', ( #11592 ) ) ;
#17749 = EDGE_CURVE ( 'NONE', #11926, #2448, #16519, .T. ) ;
#17750 = VERTEX_POINT ( 'NONE', #18062 ) ;
#17751 = CARTESIAN_POINT ( 'NONE',  ( -0.5999999999999999778, 7.347880794884128857E-17, 7.599999999999999645 ) ) ;
#17752 = VECTOR ( 'NONE', #16084, 1000.000000000000000 ) ;
#17753 = FACE_OUTER_BOUND ( 'NONE', #13087, .T. ) ;
#17754 = ORIENTED_EDGE ( 'NONE', *, *, #8662, .F. ) ;
#17755 = CARTESIAN_POINT ( 'NONE',  ( 0.9719602541832789155, -2.844656138396589817, 6.843370931913530519 ) ) ;
#17756 = DIRECTION ( 'NONE',  ( -1.000000000000000000, 1.480297366166869931E-15, 0.000000000000000000 ) ) ;
#17757 = CARTESIAN_POINT ( 'NONE',  ( -0.5889081234606770021, -5.462076271186440124, 6.978529000034869867 ) ) ;
#17758 = FACE_OUTER_BOUND ( 'NONE', #7188, .T. ) ;
#17759 = CARTESIAN_POINT ( 'NONE',  ( -0.2023972492402590084, -2.146007489747939978, 2.355265251465770149 ) ) ;
#17760 = DIRECTION ( 'NONE',  ( -1.000000000000000000, 0.000000000000000000, 6.123233995736769734E-17 ) ) ;
#17761 = CARTESIAN_POINT ( 'NONE',  ( -1.079900583135680714, -2.029566048306499670, 2.953942563037710300 ) ) ;
#17762 = CARTESIAN_POINT ( 'NONE',  ( -0.1749999999999999889, 7.700000000000000178, 0.4000000000000000222 ) ) ;
#17763 = DIRECTION ( 'NONE',  ( -0.2721173643531200059, 0.9622640697945191723, 0.000000000000000000 ) ) ;
#17764 = VERTEX_POINT ( 'NONE', #3912 ) ;
#17765 = CARTESIAN_POINT ( 'NONE',  ( 1.569888143820300064, -0.7356046962096609576, 3.119244292431920140 ) ) ;
#17766 = EDGE_CURVE ( 'NONE', #6049, #13978, #12256, .T. ) ;
#17767 = CARTESIAN_POINT ( 'NONE',  ( -0.5999999999999999778, 11.40000000000000036, 7.599999999999999645 ) ) ;
#17768 = CARTESIAN_POINT ( 'NONE',  ( 1.728413393879709936, -4.311818300558750039, 6.297289212178290185 ) ) ;
#17769 = ORIENTED_EDGE ( 'NONE', *, *, #2305, .F. ) ;
#17770 = EDGE_LOOP ( 'NONE', ( #13835, #4103, #2885, #527 ) ) ;
#17771 = EDGE_LOOP ( 'NONE', ( #156, #7461, #9891, #6224 ) ) ;
#17772 = CARTESIAN_POINT ( 'NONE',  ( 2.500000000000000000, 3.500000000000000000, 0.6099999999999999867 ) ) ;
#17773 = CONTEXT_DEPENDENT_SHAPE_REPRESENTATION ( #17836, #16896 ) ;
#17774 = CARTESIAN_POINT ( 'NONE',  ( 1.811729841638690219, -5.041949152542369639, 3.197954009834290012 ) ) ;
#17775 = LINE ( 'NONE', #16501, #7017 ) ;
#17776 = CARTESIAN_POINT ( 'NONE',  ( 0.9499999999999999556, 2.299999999999999822, 7.700000000000000178 ) ) ;
#17777 = CARTESIAN_POINT ( 'NONE',  ( -2.190084968185500358, -1.567641158900710208, 3.838447030292489792 ) ) ;
#17778 = CARTESIAN_POINT ( 'NONE',  ( 1.550000000000000044, -5.599999999999999645, 6.100000000000000533 ) ) ;
#17779 = CARTESIAN_POINT ( 'NONE',  ( -1.417606053559450352, -4.707719201459645397, 6.185023541745952258 ) ) ;
#17780 = CARTESIAN_POINT ( 'NONE',  ( 0.3743405594629510280, -0.1423728813559329842, 7.023440622744399953 ) ) ;
#17781 = VERTEX_POINT ( 'NONE', #5211 ) ;
#17782 = CARTESIAN_POINT ( 'NONE',  ( -1.562863241354461641, -0.4913135593220345210, 6.031217337312382298 ) ) ;
#17783 = CARTESIAN_POINT ( 'NONE',  ( 0.6493550500446280127, -0.01334745762711890028, 2.437955526623099889 ) ) ;
#17784 = ORIENTED_EDGE ( 'NONE', *, *, #10277, .F. ) ;
#17785 = CARTESIAN_POINT ( 'NONE',  ( -1.889104232906369862, -5.555508474576269506, 3.296507079072529933 ) ) ;
#17786 = DIRECTION ( 'NONE',  ( 0.000000000000000000, -1.000000000000000000, 0.000000000000000000 ) ) ;
#17787 = CARTESIAN_POINT ( 'NONE',  ( -1.305383194095490307, -0.5672554343907051377, 3.106059597508353143 ) ) ;
#17788 = CARTESIAN_POINT ( 'NONE',  ( 1.648422021521518621, -0.9155690868286361361, 6.779860219333207816 ) ) ;
#17789 = ORIENTED_EDGE ( 'NONE', *, *, #1276, .F. ) ;
#17790 = CARTESIAN_POINT ( 'NONE',  ( -1.053623506755599459, -4.865515740159335856, 2.921978671571880515 ) ) ;
#17791 = CIRCLE ( 'NONE', #10136, 0.8000000000000000444 ) ;
#17792 = CARTESIAN_POINT ( 'NONE',  ( 1.854177340199709922, -3.989623140882689434, 6.149404042554680316 ) ) ;
#17793 = CARTESIAN_POINT ( 'NONE',  ( -2.408279507600840308, -4.800872354612795156, 5.815035204050404971 ) ) ;
#17794 = CARTESIAN_POINT ( 'NONE',  ( 2.500000000000000000, 2.799999999999999822, 0.6099999999999999867 ) ) ;
#17795 = CARTESIAN_POINT ( 'NONE',  ( 0.9123513484651973870, -3.547145663405211646, 2.860838000723751051 ) ) ;
#17796 = DIRECTION ( 'NONE',  ( 9.251858538542969116E-17, 0.000000000000000000, 1.000000000000000000 ) ) ;
#17797 = DIRECTION ( 'NONE',  ( 0.7071067811865470176, 0.000000000000000000, -0.7071067811865480168 ) ) ;
#17798 = CARTESIAN_POINT ( 'NONE',  ( 2.051695471449629160, -2.266289807549351387, 4.773807418740724451 ) ) ;
#17799 = ORIENTED_EDGE ( 'NONE', *, *, #4754, .F. ) ;
#17800 = LINE ( 'NONE', #5137, #12805 ) ;
#17801 = DIRECTION ( 'NONE',  ( -1.000000000000000000, -3.172065784643300034E-16, -2.220446049250309876E-16 ) ) ;
#17802 = CARTESIAN_POINT ( 'NONE',  ( 1.741105240696918965, -0.4774152569121725143, 2.691996915772988608 ) ) ;
#17803 = CARTESIAN_POINT ( 'NONE',  ( 2.161103922260819044, -2.103271789531340641, 3.159628768708413915 ) ) ;
#17804 = ORIENTED_EDGE ( 'NONE', *, *, #701, .T. ) ;
#17805 = CARTESIAN_POINT ( 'NONE',  ( 1.899999999999999911, 0.5999999999999999778, 1.600000000000000089 ) ) ;
#17806 = CARTESIAN_POINT ( 'NONE',  ( 3.179896940101190659E-17, 3.786446520921929793, 7.919316580472860245 ) ) ;
#17807 = CARTESIAN_POINT ( 'NONE',  ( 1.641808337277750107, -5.113135593220339281, 6.386111670537619744 ) ) ;
#17808 = VERTEX_POINT ( 'NONE', #4102 ) ;
#17809 = EDGE_LOOP ( 'NONE', ( #6466, #8012, #12097, #12470, #1914, #2790, #8723, #1494, #12181, #17617, #2729, #11350, #10597, #5950, #17799, #214, #18044, #2815, #4987, #4343, #7746, #17865, #2522, #15247, #17555, #13458, #9243, #2810 ) ) ;
#17810 = DIRECTION ( 'NONE',  ( 0.000000000000000000, -1.000000000000000000, 0.000000000000000000 ) ) ;
#17811 = CARTESIAN_POINT ( 'NONE',  ( 0.3750000000000000000, 3.050000000000000266, 2.100000000000000089 ) ) ;
#17812 = PLANE ( 'NONE',  #4347 ) ;
#17813 = ORIENTED_EDGE ( 'NONE', *, *, #11051, .F. ) ;
#17814 = CARTESIAN_POINT ( 'NONE',  ( -1.707817112497179934, -5.488771186440679628, 6.319218296629480314 ) ) ;
#17815 = CARTESIAN_POINT ( 'NONE',  ( -2.418933091173281369, -4.501965483225034426, 5.791730916219171021 ) ) ;
#17816 = DIRECTION ( 'NONE',  ( 0.000000000000000000, 0.000000000000000000, -1.000000000000000000 ) ) ;
#17817 = CARTESIAN_POINT ( 'NONE',  ( -2.652303127816829864, -3.333710192450643373, 4.791661394135809715 ) ) ;
#17818 = CARTESIAN_POINT ( 'NONE',  ( -2.200000000000000178, -2.672352773677590478E-16, 4.000000000000000000 ) ) ;
#17819 = DIRECTION ( 'NONE',  ( 1.224646799147349263E-16, 0.000000000000000000, 1.000000000000000000 ) ) ;
#17820 = CARTESIAN_POINT ( 'NONE',  ( -2.145694642186069867, -4.501965483225029985, 5.666819626392589626 ) ) ;
#17821 = ADVANCED_FACE ( 'NONE', ( #4001 ), #962, .T. ) ;
#17822 = PLANE ( 'NONE',  #2030 ) ;
#17824 = ORIENTED_EDGE ( 'NONE', *, *, #13839, .T. ) ;
#17823 = CARTESIAN_POINT ( 'NONE',  ( 2.635341251434490495, -2.588484967225421762, 5.013193520829454464 ) ) ;
#17825 = ADVANCED_FACE ( 'NONE', ( #1055 ), #6693, .F. ) ;
#17826 = EDGE_CURVE ( 'NONE', #8528, #1801, #11044, .T. ) ;
#17827 = DIRECTION ( 'NONE',  ( -2.220446049250309876E-16, 1.000000000000000000, 0.000000000000000000 ) ) ;
#17828 = CARTESIAN_POINT ( 'NONE',  ( 1.428515267734870031, -0.3311440677966109858, 2.829745655876919841 ) ) ;
#17829 = CARTESIAN_POINT ( 'NONE',  ( 1.764807890102179977, -2.378890372630820149, 3.143016121304719857 ) ) ;
#17830 = CARTESIAN_POINT ( 'NONE',  ( 0.009451942938126131968, -5.000194708068004701, 2.339951117923973367 ) ) ;
#17831 = DIRECTION ( 'NONE',  ( 0.000000000000000000, -1.000000000000000000, 0.000000000000000000 ) ) ;
#17832 = CARTESIAN_POINT ( 'NONE',  ( -1.889104232906369862, -5.555508474576269506, 3.296507079072529933 ) ) ;
#17833 = ORIENTED_EDGE ( 'NONE', *, *, #2363, .T. ) ;
#17834 = FACE_OUTER_BOUND ( 'NONE', #2420, .T. ) ;
#17835 = CARTESIAN_POINT ( 'NONE',  ( 1.890000000000029878, 4.100000000000000533, 3.000000000000000000 ) ) ;
#17836 =( REPRESENTATION_RELATIONSHIP ('NONE','NONE', #2757, #2146 ) REPRESENTATION_RELATIONSHIP_WITH_TRANSFORMATION ( #13348 )SHAPE_REPRESENTATION_RELATIONSHIP( ) );
#17837 = EDGE_LOOP ( 'NONE', ( #15960, #16043, #9705 ) ) ;
#17838 = CARTESIAN_POINT ( 'NONE',  ( 2.100188519621589922, -4.009070552810999999, 3.637948273607370275 ) ) ;
#17839 = EDGE_CURVE ( 'NONE', #1588, #8456, #8283, .T. ) ;
#17840 = CARTESIAN_POINT ( 'NONE',  ( -0.3042893218813459977, 6.450000000000000178, 2.029289321881350361 ) ) ;
#17841 = FACE_OUTER_BOUND ( 'NONE', #5318, .T. ) ;
#17842 = CIRCLE ( 'NONE', #12251, 0.4000000000000001887 ) ;
#17843 = LINE ( 'NONE', #2129, #13181 ) ;
#17844 = EDGE_CURVE ( 'NONE', #13844, #11906, #5320, .T. ) ;
#17845 = PLANE ( 'NONE',  #15876 ) ;
#17846 = CARTESIAN_POINT ( 'NONE',  ( -1.145304265383870090, -3.077539021279469988, 6.755972720436099088 ) ) ;
#17847 = DIRECTION ( 'NONE',  ( 6.123233995736823968E-17, 0.000000000000000000, 1.000000000000000000 ) ) ;
#17848 = CARTESIAN_POINT ( 'NONE',  ( 1.764143222953819867, -2.425466949207401690, 3.649904513135025841 ) ) ;
#17849 = CARTESIAN_POINT ( 'NONE',  ( 0.5500000000000000444, 6.450000000000000178, 1.600000000000000089 ) ) ;
#17850 = CARTESIAN_POINT ( 'NONE',  ( -1.221947981261169991, -0.5741044150835520332, 2.670403636935529956 ) ) ;
#17851 = ORIENTED_EDGE ( 'NONE', *, *, #5415, .T. ) ;
#17852 = CARTESIAN_POINT ( 'NONE',  ( -1.899999999999999911, 11.40000000000000036, 1.600000000000000089 ) ) ;
#17853 = PLANE ( 'NONE',  #11928 ) ;
#17854 = CARTESIAN_POINT ( 'NONE',  ( -2.065623031241579977, -5.033755237495680213, 3.572193642975310279 ) ) ;
#17855 = CIRCLE ( 'NONE', #12860, 0.5999999999999998668 ) ;
#17856 = ORIENTED_EDGE ( 'NONE', *, *, #2569, .T. ) ;
#17857 = ORIENTED_EDGE ( 'NONE', *, *, #10271, .F. ) ;
#17858 = DIRECTION ( 'NONE',  ( -1.000000000000000000, 0.000000000000000000, 0.000000000000000000 ) ) ;
#17859 = PRODUCT_DEFINITION_CONTEXT ( 'detailed design', #2003, 'design' ) ;
#17860 = VERTEX_POINT ( 'NONE', #15325 ) ;
#17861 = DIRECTION ( 'NONE',  ( 1.224646799147350002E-16, -1.000000000000000000, -6.123233995736769734E-17 ) ) ;
#17862 = CARTESIAN_POINT ( 'NONE',  ( 0.7093417302541469294, -5.135381355932199909, 6.943956659919690466 ) ) ;
#17863 = EDGE_CURVE ( 'NONE', #12165, #6842, #10772, .T. ) ;
#17864 = LINE ( 'NONE', #1043, #9424 ) ;
#17865 = ORIENTED_EDGE ( 'NONE', *, *, #9242, .F. ) ;
#17866 = CARTESIAN_POINT ( 'NONE',  ( 0.2564439965879030114, -1.055298816558370101, 7.039440566481209416 ) ) ;
#17867 = ADVANCED_FACE ( 'NONE', ( #10867 ), #16415, .T. ) ;
#17868 = PLANE ( 'NONE',  #16774 ) ;
#17869 = CARTESIAN_POINT ( 'NONE',  ( -1.381042549632419902, -1.540511994252449890, 6.605640880016140137 ) ) ;
#17870 = CARTESIAN_POINT ( 'NONE',  ( -2.586172839791708533, -0.2358050847457631438, 4.104546363490954697 ) ) ;
#17871 = ORIENTED_EDGE ( 'NONE', *, *, #1328, .T. ) ;
#17872 = ORIENTED_EDGE ( 'NONE', *, *, #8010, .T. ) ;
#17873 = CARTESIAN_POINT ( 'NONE',  ( 0.5000000000000000000, 4.631370849898480024, 6.100000000000000533 ) ) ;
#17874 = CARTESIAN_POINT ( 'NONE',  ( -2.500000000000000000, 2.000000000000000000, 1.600000000000000089 ) ) ;
#17875 = PLANE ( 'NONE',  #4085 ) ;
#17876 = CARTESIAN_POINT ( 'NONE',  ( -2.342931736853879787, -1.497776294035839895, 4.477701633099188783 ) ) ;
#17877 =( NAMED_UNIT ( * ) PLANE_ANGLE_UNIT ( ) SI_UNIT ( $, .RADIAN. ) );
#17878 = CARTESIAN_POINT ( 'NONE',  ( -1.066267773695860122, -0.5741044150835525883, 2.929718414487351374 ) ) ;
#17879 = CARTESIAN_POINT ( 'NONE',  ( -1.882879255550339082, -5.103620102360555855, 2.835213315261639000 ) ) ;
#17880 = EDGE_LOOP ( 'NONE', ( #14641, #16133, #1327, #17324 ) ) ;
#17881 = CARTESIAN_POINT ( 'NONE',  ( -1.440522616026439495, -4.804713230972779137, 3.241384813161591438 ) ) ;
#17882 = CARTESIAN_POINT ( 'NONE',  ( -0.2818998297622349880, -4.245794312053860153, 7.036509827384409554 ) ) ;
#17883 = CARTESIAN_POINT ( 'NONE',  ( 2.248786803694151182, -4.265241723982168942, 6.109280527266637506 ) ) ;
#17884 = ADVANCED_FACE ( 'NONE', ( #15139 ), #8375, .T. ) ;
#17885 = CARTESIAN_POINT ( 'NONE',  ( -1.889999999999999902, 7.299999999999999822, 0.5999999999999999778 ) ) ;
#17886 = CARTESIAN_POINT ( 'NONE',  ( 0.1749999999999999889, 9.500000000000000000, 3.100000000000000089 ) ) ;
#17887 = CARTESIAN_POINT ( 'NONE',  ( -1.842787987253248883, -1.889836318576769036, 3.794994874786233652 ) ) ;
#17888 = CARTESIAN_POINT ( 'NONE',  ( -4.898587196589400133E-17, 5.318248954186070243, 6.599999999999999645 ) ) ;
#17889 = DIRECTION ( 'NONE',  ( 8.997169018144999103E-17, -9.633757521571540356E-31, -1.000000000000000000 ) ) ;
#17890 = CARTESIAN_POINT ( 'NONE',  ( 2.052909741356249373, -3.826605122864674247, 4.721527574705135066 ) ) ;
#17891 = ORIENTED_EDGE ( 'NONE', *, *, #13244, .F. ) ;
#17892 = CARTESIAN_POINT ( 'NONE',  ( 0.000000000000000000, 0.000000000000000000, 8.300000000000000711 ) ) ;
#17893 = CARTESIAN_POINT ( 'NONE',  ( 1.899999999999999911, 2.000000000000000000, 1.600000000000000089 ) ) ;
#17894 = AXIS2_PLACEMENT_3D ( 'NONE', #7306, #5920, #12954 ) ;
#17895 = CARTESIAN_POINT ( 'NONE',  ( 0.1749999999999999889, 7.500000000000000000, 1.600000000000000089 ) ) ;
#17896 = CARTESIAN_POINT ( 'NONE',  ( -1.901407128523849632, -2.848497014756559143, 6.551422324754827109 ) ) ;
#17897 = VERTEX_POINT ( 'NONE', #9568 ) ;
#17898 = AXIS2_PLACEMENT_3D ( 'NONE', #5181, #16202, #16476 ) ;
#17899 = FACE_BOUND ( 'NONE', #10305, .T. ) ;
#17900 = LINE ( 'NONE', #13673, #1200 ) ;
#17901 = CARTESIAN_POINT ( 'NONE',  ( -0.1910247150515231307, -5.295550847457634269, 2.655937705488500722 ) ) ;
#17902 = ORIENTED_EDGE ( 'NONE', *, *, #14944, .T. ) ;
#17903 = ORIENTED_EDGE ( 'NONE', *, *, #9808, .F. ) ;
#17904 = DIRECTION ( 'NONE',  ( 0.000000000000000000, 0.000000000000000000, 1.000000000000000000 ) ) ;
#17905 = CARTESIAN_POINT ( 'NONE',  ( 1.300000000000000044, -1.592040838891560081E-16, 7.599999999999999645 ) ) ;
#17906 = CARTESIAN_POINT ( 'NONE',  ( 1.983927814618709873E-15, 10.80000000000000071, 8.599999999999999645 ) ) ;
#17907 = ORIENTED_EDGE ( 'NONE', *, *, #7336, .T. ) ;
#17908 = CARTESIAN_POINT ( 'NONE',  ( -1.978267656359410154, -5.497669491525420504, 5.974740860598790171 ) ) ;
#17909 = CARTESIAN_POINT ( 'NONE',  ( 2.380466601827069262, -3.710163681423226389, 3.526759849567131955 ) ) ;
#17910 = CARTESIAN_POINT ( 'NONE',  ( -1.449852972480019764, -3.589881363621813648, 2.477154964647171109 ) ) ;
#17911 = VECTOR ( 'NONE', #2053, 1000.000000000000000 ) ;
#17912 = CARTESIAN_POINT ( 'NONE',  ( -0.1749999999999999889, 7.500000000000000000, 3.100000000000000089 ) ) ;
#17913 = CARTESIAN_POINT ( 'NONE',  ( 1.417606053559480328, -0.8922807985403484743, 6.185023541745921172 ) ) ;
#17914 = CARTESIAN_POINT ( 'NONE',  ( 1.000000000000000000, -8.000000000000000000, 5.700000000000000178 ) ) ;
#17915 = DIRECTION ( 'NONE',  ( 1.000000000000000000, 0.000000000000000000, 0.000000000000000000 ) ) ;
#17917 = ORIENTED_EDGE ( 'NONE', *, *, #4124, .F. ) ;
#17916 = CARTESIAN_POINT ( 'NONE',  ( -0.6015868932279860859, -3.007674156414608557, 7.284803068494427158 ) ) ;
#17918 = VECTOR ( 'NONE', #11650, 1000.000000000000000 ) ;
#17919 = CYLINDRICAL_SURFACE ( 'NONE', #10019, 0.6500000000000003553 ) ;
#17920 = CARTESIAN_POINT ( 'NONE',  ( 2.253200202764420013, -0.3889830508474579895, 5.379408587037500133 ) ) ;
#17921 = CARTESIAN_POINT ( 'NONE',  ( -0.2023972492402590084, -2.146007489747939978, 2.355265251465770149 ) ) ;
#17922 = AXIS2_PLACEMENT_3D ( 'NONE', #16682, #15578, #11400 ) ;
#17923 = CARTESIAN_POINT ( 'NONE',  ( -1.800000000000000044, 11.40000000000000036, 7.550000000000000711 ) ) ;
#17924 = DIRECTION ( 'NONE',  ( -0.7071067811865474617, 0.000000000000000000, -0.7071067811865474617 ) ) ;
#17925 = CARTESIAN_POINT ( 'NONE',  ( 1.873832970144350130, -5.337500000000000355, 2.826167029855650270 ) ) ;
#17926 = ORIENTED_EDGE ( 'NONE', *, *, #1276, .T. ) ;
#17927 = LINE ( 'NONE', #16570, #16689 ) ;
#17928 = AXIS2_PLACEMENT_3D ( 'NONE', #110, #9743, #5757 ) ;
#17929 = VERTEX_POINT ( 'NONE', #2450 ) ;
#17930 = CARTESIAN_POINT ( 'NONE',  ( 2.332582362116870200, -5.068644067796608255, 4.387643303570811781 ) ) ;
#17931 = DIRECTION ( 'NONE',  ( 0.000000000000000000, -1.000000000000000000, 0.000000000000000000 ) ) ;
#17932 = CARTESIAN_POINT ( 'NONE',  ( -0.0009602353114164120101, -0.4652189165859030306, 2.501032900279570370 ) ) ;
#17933 = PRODUCT_DEFINITION ( 'UNKNOWN', '', #10623, #3810 ) ;
#17934 = VERTEX_POINT ( 'NONE', #2531 ) ;
#17935 = ADVANCED_FACE ( 'NONE', ( #3721 ), #8180, .T. ) ;
#17936 = VECTOR ( 'NONE', #440, 1000.000000000000000 ) ;
#17937 = CARTESIAN_POINT ( 'NONE',  ( -1.917298190932639868, -3.496728210468659892, 3.335187436117939885 ) ) ;
#17938 = PLANE ( 'NONE',  #18223 ) ;
#17939 = CARTESIAN_POINT ( 'NONE',  ( 2.023259452208809872, -2.425466949207399914, 3.497849062500220096 ) ) ;
#17940 = AXIS2_PLACEMENT_3D ( 'NONE', #10625, #14887, #17819 ) ;
#17941 = CARTESIAN_POINT ( 'NONE',  ( -2.296954468777729463, -4.963890372630819670, 4.187412587068699565 ) ) ;
#17942 = CARTESIAN_POINT ( 'NONE',  ( 0.7616804549307097938, -2.262448931189378509, 2.793499350326721142 ) ) ;
#17943 = FACE_OUTER_BOUND ( 'NONE', #5748, .T. ) ;
#17944 = VECTOR ( 'NONE', #862, 1000.000000000000000 ) ;
#17945 = AXIS2_PLACEMENT_3D ( 'NONE', #4641, #7441, #1953 ) ;
#17946 = ORIENTED_EDGE ( 'NONE', *, *, #9405, .F. ) ;
#17947 = EDGE_CURVE ( 'NONE', #8985, #8650, #12444, .T. ) ;
#17948 = DIRECTION ( 'NONE',  ( -7.401486830834380223E-16, -1.000000000000000000, 0.000000000000000000 ) ) ;
#17949 = CARTESIAN_POINT ( 'NONE',  ( -2.135041058613629694, -4.800872354612799597, 5.690123914223820023 ) ) ;
#17950 = EDGE_LOOP ( 'NONE', ( #3370, #15422, #1610, #10981 ) ) ;
#17951 = EDGE_LOOP ( 'NONE', ( #3261, #1013, #14207, #16369 ) ) ;
#17952 = EDGE_CURVE ( 'NONE', #1650, #10646, #13923, .T. ) ;
#17953 = VECTOR ( 'NONE', #9867, 1000.000000000000000 ) ;
#17954 = ORIENTED_EDGE ( 'NONE', *, *, #12319, .T. ) ;
#17955 = DIRECTION ( 'NONE',  ( 0.000000000000000000, 0.000000000000000000, 1.000000000000000000 ) ) ;
#17956 = EDGE_CURVE ( 'NONE', #12938, #2115, #16811, .T. ) ;
#17957 = CARTESIAN_POINT ( 'NONE',  ( 0.06264882350516240428, -5.148728813559320550, 7.052569299041220319 ) ) ;
#17958 = CARTESIAN_POINT ( 'NONE',  ( -0.6500000000000000222, 6.450000000000000178, 2.699264068711930253 ) ) ;
#17959 = AXIS2_PLACEMENT_3D ( 'NONE', #2323, #7972, #3884 ) ;
#17960 = CARTESIAN_POINT ( 'NONE',  ( 1.000000000000000000, -5.500000000000000000, 5.100000000000000533 ) ) ;
#17961 = CARTESIAN_POINT ( 'NONE',  ( 2.218077401483169897, -0.7758393570989060573, 5.486688202856499608 ) ) ;
#17962 = AXIS2_PLACEMENT_3D ( 'NONE', #12853, #5908, #11549 ) ;
#17963 = CARTESIAN_POINT ( 'NONE',  ( 1.889999999999999902, 8.500000000000000000, 0.6099999999999999867 ) ) ;
#17964 = CARTESIAN_POINT ( 'NONE',  ( 2.287919158821199783, -1.051457940198389895, 5.251517552016890633 ) ) ;
#17965 = CARTESIAN_POINT ( 'NONE',  ( 1.978267656359410154, -0.1023305084745769894, 5.974740860598790171 ) ) ;
#17966 = VECTOR ( 'NONE', #17673, 1000.000000000000000 ) ;
#17967 = VERTEX_POINT ( 'NONE', #5490 ) ;
#17968 = CARTESIAN_POINT ( 'NONE',  ( -2.058670345754650022, -0.5491525423728820243, 3.559656372813929881 ) ) ;
#17969 = ORIENTED_EDGE ( 'NONE', *, *, #9808, .T. ) ;
#17970 = ADVANCED_FACE ( 'NONE', ( #1323 ), #11132, .T. ) ;
#17971 = CARTESIAN_POINT ( 'NONE',  ( 0.4221287159901364605, -0.1423728813559330397, 7.320050063945812369 ) ) ;
#17972 = ORIENTED_EDGE ( 'NONE', *, *, #2035, .F. ) ;
#17973 = CIRCLE ( 'NONE', #12677, 0.4999999999999995559 ) ;
#17974 = VECTOR ( 'NONE', #13782, 1000.000000000000000 ) ;
#17975 = DIRECTION ( 'NONE',  ( 0.000000000000000000, 0.000000000000000000, -1.000000000000000000 ) ) ;
#17976 = ADVANCED_FACE ( 'NONE', ( #4372 ), #217, .F. ) ;
#17977 = CARTESIAN_POINT ( 'NONE',  ( -1.526791597786389287, -2.825208726468270370, 6.490992212270281669 ) ) ;
#17978 = CARTESIAN_POINT ( 'NONE',  ( -2.116444151961480280, -5.546610169491529518, 3.670839500609359707 ) ) ;
#17979 = CARTESIAN_POINT ( 'NONE',  ( -2.622715975066178817, -4.870737219477664581, 5.105554690683034913 ) ) ;
#17980 = ORIENTED_EDGE ( 'NONE', *, *, #3500, .T. ) ;
#17981 = CARTESIAN_POINT ( 'NONE',  ( -1.074005996636800075, -5.164643153926310681, 2.934052701886380010 ) ) ;
#17982 = CARTESIAN_POINT ( 'NONE',  ( 2.051973656473811136, -0.6826862039457533005, 4.634380218157459375 ) ) ;
#17983 = CARTESIAN_POINT ( 'NONE',  ( -2.159308672244651284, -4.754295778036219389, 6.242886823772542115 ) ) ;
#17984 = CARTESIAN_POINT ( 'NONE',  ( 2.500000000000000000, 11.15000000000000036, 1.600000000000000089 ) ) ;
#17985 = DIRECTION ( 'NONE',  ( 0.000000000000000000, -1.000000000000000000, 0.000000000000000000 ) ) ;
#17986 = VECTOR ( 'NONE', #6350, 1000.000000000000000 ) ;
#17987 = CARTESIAN_POINT ( 'NONE',  ( 0.4365326870214371602, -1.330917399657850497, 6.706076034398976482 ) ) ;
#17988 = DIRECTION ( 'NONE',  ( 0.000000000000000000, 0.000000000000000000, -1.000000000000000000 ) ) ;
#17989 = EDGE_CURVE ( 'NONE', #4730, #7436, #17138, .T. ) ;
#17990 = VERTEX_POINT ( 'NONE', #10193 ) ;
#17991 = DIRECTION ( 'NONE',  ( -0.7071067811865480168, 0.7071067811865470176, 0.000000000000000000 ) ) ;
#17992 = CARTESIAN_POINT ( 'NONE',  ( -11.62823001646920140, -7.413791402719209319E-16, 0.5999999999999698908 ) ) ;
#17993 = CARTESIAN_POINT ( 'NONE',  ( 1.754713504580569960, -0.3489406779661023417, 3.634325740584615883 ) ) ;
#17994 = CARTESIAN_POINT ( 'NONE',  ( -1.370891210199559618, -1.730659176918718956, 2.427606771969371469 ) ) ;
#17995 = EDGE_LOOP ( 'NONE', ( #12898, #15874, #2959, #11779, #14745, #16308, #12729, #6651 ) ) ;
#17996 = CARTESIAN_POINT ( 'NONE',  ( -1.800000000000000044, 0.5999999999999999778, 7.550000000000000711 ) ) ;
#17997 = CARTESIAN_POINT ( 'NONE',  ( 2.000624272291700034, -5.364194915254235418, 4.239366054775996595 ) ) ;
#17998 = VERTEX_POINT ( 'NONE', #10034 ) ;
#17999 = EDGE_CURVE ( 'NONE', #16239, #17967, #3081, .T. ) ;
#18000 = LINE ( 'NONE', #9592, #5643 ) ;
#18001 = DIRECTION ( 'NONE',  ( 2.242874797222529735E-16, 0.000000000000000000, 1.000000000000000000 ) ) ;
#18002 = CIRCLE ( 'NONE', #8850, 1.016666666666670160 ) ;
#18003 = FACE_OUTER_BOUND ( 'NONE', #10857, .T. ) ;
#18004 = ORIENTED_EDGE ( 'NONE', *, *, #14561, .T. ) ;
#18005 = CARTESIAN_POINT ( 'NONE',  ( 1.641808337277750107, -5.413135593220339103, 6.386111670537619744 ) ) ;
#18006 = CARTESIAN_POINT ( 'NONE',  ( 0.4247583764261176897, -4.175929447188994281, 7.319674410047496416 ) ) ;
#18007 = DIRECTION ( 'NONE',  ( 0.000000000000000000, 0.000000000000000000, -1.000000000000000000 ) ) ;
#18008 = CARTESIAN_POINT ( 'NONE',  ( 1.802718065953961002, -0.5662447625043125488, 3.717600174934180046 ) ) ;
#18009 = DIRECTION ( 'NONE',  ( 1.807003620809174583E-15, 1.000000000000000000, 1.807003620809174385E-16 ) ) ;
#18010 = PLANE ( 'NONE',  #8265 ) ;
#18011 = ORIENTED_EDGE ( 'NONE', *, *, #12083, .F. ) ;
#18012 = VECTOR ( 'NONE', #3497, 1000.000000000000000 ) ;
#18013 = CARTESIAN_POINT ( 'NONE',  ( 1.766091042938769951, -5.222834417938730489, 2.933908957061230005 ) ) ;
#18014 = CARTESIAN_POINT ( 'NONE',  ( 1.192209327851080136, -0.3222457627118649470, 2.329031440774910422 ) ) ;
#18015 = CARTESIAN_POINT ( 'NONE',  ( -1.710920205120030069, -1.587088570829020107, 6.316012914303580139 ) ) ;
#18016 = CARTESIAN_POINT ( 'NONE',  ( 2.500000000000000000, 9.199999999999999289, 1.600000000000000089 ) ) ;
#18017 = DIRECTION ( 'NONE',  ( 0.000000000000000000, -1.000000000000000000, 0.000000000000000000 ) ) ;
#18018 = CARTESIAN_POINT ( 'NONE',  ( -0.1765068388402301069, -5.453177966101685037, 7.347961541693632803 ) ) ;
#18019 = VERTEX_POINT ( 'NONE', #8724 ) ;
#18020 = DIRECTION ( 'NONE',  ( -1.644774851296529842E-16, 1.000000000000000000, 0.000000000000000000 ) ) ;
#18021 = VERTEX_POINT ( 'NONE', #11330 ) ;
#18022 = CARTESIAN_POINT ( 'NONE',  ( -1.549742865090599997, -5.184322033898308923, 6.471102547561461193 ) ) ;
#18023 = DIRECTION ( 'NONE',  ( 0.000000000000000000, 0.000000000000000000, 1.000000000000000000 ) ) ;
#18024 = CARTESIAN_POINT ( 'NONE',  ( 1.899999999999999911, 3.500000000000000000, 0.6099999999999999867 ) ) ;
#18025 = EDGE_LOOP ( 'NONE', ( #7293, #1284, #8148, #18135 ) ) ;
#18026 = VECTOR ( 'NONE', #17529, 1000.000000000000000 ) ;
#18027 = ADVANCED_FACE ( 'NONE', ( #1423 ), #5949, .T. ) ;
#18028 = CARTESIAN_POINT ( 'NONE',  ( -0.03714311608457869507, -4.521412895153340550, 7.053160869216429596 ) ) ;
#18029 = ADVANCED_FACE ( 'NONE', ( #8821 ), #14473, .F. ) ;
#18030 = CARTESIAN_POINT ( 'NONE',  ( 1.307725206348619995, -0.7471169921413569615, 2.732408283416570161 ) ) ;
#18031 = CARTESIAN_POINT ( 'NONE',  ( -0.009452110982655114943, -5.299807955295455564, 2.050000000000001155 ) ) ;
#18032 = CARTESIAN_POINT ( 'NONE',  ( -1.599999999999869971, 12.00000000000000000, -2.399999999999999911 ) ) ;
#18033 = CARTESIAN_POINT ( 'NONE',  ( -1.800000000000000044, 0.5999999999999999778, 7.599999999999999645 ) ) ;
#18034 = CARTESIAN_POINT ( 'NONE',  ( 1.074829861819710075, -2.285737219477669946, 2.606322265575589991 ) ) ;
#18035 = DIRECTION ( 'NONE',  ( -2.168404344971009262E-15, -1.000000000000000000, -2.220446049250220143E-16 ) ) ;
#18036 = CARTESIAN_POINT ( 'NONE',  ( 1.404946080800569375, -2.355602084342530933, 3.202993536195909208 ) ) ;
#18037 = DIRECTION ( 'NONE',  ( -4.440892098500630895E-15, 1.000000000000000000, 0.000000000000000000 ) ) ;
#18038 = AXIS2_PLACEMENT_3D ( 'NONE', #15080, #8208, #15251 ) ;
#18039 = CARTESIAN_POINT ( 'NONE',  ( -0.1926573868394080846, -0.2965485159365558454, 2.049233193116839935 ) ) ;
#18040 = ORIENTED_EDGE ( 'NONE', *, *, #15933, .T. ) ;
#18041 = DIRECTION ( 'NONE',  ( 1.110223024625159992E-16, 0.000000000000000000, -1.000000000000000000 ) ) ;
#18042 = CARTESIAN_POINT ( 'NONE',  ( -1.722199153441400066, -5.095857339597789526, 3.099360556065549943 ) ) ;
#18043 = ORIENTED_EDGE ( 'NONE', *, *, #6779, .T. ) ;
#18044 = ORIENTED_EDGE ( 'NONE', *, *, #14920, .F. ) ;
#18045 = ORIENTED_EDGE ( 'NONE', *, *, #16496, .T. ) ;
#18046 = CARTESIAN_POINT ( 'NONE',  ( 1.875000000000000000, -2.296212748401290437E-16, 7.700000000000000178 ) ) ;
#18047 = CARTESIAN_POINT ( 'NONE',  ( 1.432215783582721613, -5.113135593220339281, 6.170863372171116801 ) ) ;
#18048 = DIRECTION ( 'NONE',  ( -2.529805069132844337E-15, 1.000000000000000000, 1.807003620809174385E-16 ) ) ;
#18049 = CARTESIAN_POINT ( 'NONE',  ( -1.000000000000000000, -8.000000000000000000, 3.700000000000000178 ) ) ;
#18050 = ADVANCED_FACE ( 'NONE', ( #395 ), #13254, .T. ) ;
#18051 = CARTESIAN_POINT ( 'NONE',  ( 2.500000000000000000, 10.00000000000000000, 0.5999999999999999778 ) ) ;
#18052 = CARTESIAN_POINT ( 'NONE',  ( -1.552749016687749783, -1.563800282540730002, 6.468535037441760061 ) ) ;
#18053 = EDGE_CURVE ( 'NONE', #14775, #12624, #9428, .T. ) ;
#18054 = CARTESIAN_POINT ( 'NONE',  ( 1.596341326794969984, -0.03559322033898330156, 2.970780074643809776 ) ) ;
#18055 = DIRECTION ( 'NONE',  ( 0.000000000000000000, 0.000000000000000000, -1.000000000000000000 ) ) ;
#18056 = EDGE_CURVE ( 'NONE', #6568, #11460, #11486, .T. ) ;
#18057 = EDGE_CURVE ( 'NONE', #2805, #6472, #16122, .T. ) ;
#18058 = ORIENTED_EDGE ( 'NONE', *, *, #12813, .T. ) ;
#18059 = CARTESIAN_POINT ( 'NONE',  ( 2.540842781840729536, -0.08898305084745804228, 5.466141598148674952 ) ) ;
#18060 = DIRECTION ( 'NONE',  ( 6.672013369141562259E-16, 0.000000000000000000, 1.000000000000000000 ) ) ;
#18061 = ORIENTED_EDGE ( 'NONE', *, *, #12779, .F. ) ;
#18062 = CARTESIAN_POINT ( 'NONE',  ( -2.500000000000000000, 7.299999999999999822, 0.6099999999999999867 ) ) ;
#18063 = CARTESIAN_POINT ( 'NONE',  ( 0.9485663501270545916, -2.545749267008809991, 6.853826262002240099 ) ) ;
#18064 = CARTESIAN_POINT ( 'NONE',  ( -1.889104232906369862, -5.555508474576269506, 3.296507079072529933 ) ) ;
#18065 = CARTESIAN_POINT ( 'NONE',  ( 2.501774541437309374, -0.7758393570989061683, 5.585572039315881199 ) ) ;
#18066 = EDGE_LOOP ( 'NONE', ( #8175, #945, #9440, #10839 ) ) ;
#18067 = LINE ( 'NONE', #16699, #6681 ) ;
#18068 = CARTESIAN_POINT ( 'NONE',  ( 1.668733558229380520, -0.8457042219637719294, 5.895922302771890777 ) ) ;
#18069 = CARTESIAN_POINT ( 'NONE',  ( 2.437122747866759198, -0.5895330507926000996, 3.649501829874934433 ) ) ;
#18070 = CARTESIAN_POINT ( 'NONE',  ( -0.1749999999999999889, 6.799999999999999822, 1.600000000000000089 ) ) ;
#18071 = CARTESIAN_POINT ( 'NONE',  ( -1.899999999999999911, 0.5999999999999999778, 7.599999999999999645 ) ) ;
#18072 = CARTESIAN_POINT ( 'NONE',  ( -1.353302556710470395, -1.563800282540731779, 6.243850391919187892 ) ) ;
#18074 = EDGE_CURVE ( 'NONE', #14528, #5861, #1948, .T. ) ;
#18073 = DIRECTION ( 'NONE',  ( 0.000000000000000000, 0.000000000000000000, 1.000000000000000000 ) ) ;
#18075 = VERTEX_POINT ( 'NONE', #14729 ) ;
#18076 = LINE ( 'NONE', #9671, #10415 ) ;
#18077 = CARTESIAN_POINT ( 'NONE',  ( 2.500000000000000000, 7.299999999999999822, 1.600000000000000089 ) ) ;
#18078 = CARTESIAN_POINT ( 'NONE',  ( -2.000624272291700034, -0.2358050847457631438, 4.239366054776020576 ) ) ;
#18079 = VECTOR ( 'NONE', #18112, 1000.000000000000000 ) ;
#18080 = B_SPLINE_CURVE_WITH_KNOTS ( 'NONE', 3,
 ( #9514, #805, #16175, #15173, #16269, #3572, #7841 ),
 .UNSPECIFIED., .F., .F.,
 ( 4, 1, 1, 1, 4 ),
 ( 0.000000000000000000, 0.3003308066894049833, 0.4325493167363730351, 0.5576349185191149527, 0.7853981633974479459 ),
 .UNSPECIFIED. ) ;
#18081 = CARTESIAN_POINT ( 'NONE',  ( 2.295344368707611160, -2.126560077819629413, 3.367893426919545519 ) ) ;
#18082 = CARTESIAN_POINT ( 'NONE',  ( -0.009452110982656913851, -5.299807955295455564, 2.050000000000001155 ) ) ;
#18083 = CARTESIAN_POINT ( 'NONE',  ( -1.980638384804660257, -5.237711864406785267, 4.159858630563765480 ) ) ;
#18084 = ORIENTED_EDGE ( 'NONE', *, *, #3475, .F. ) ;
#18085 = DIRECTION ( 'NONE',  ( -1.306144734853129823E-16, 1.000000000000000000, 0.000000000000000000 ) ) ;
#18086 = CARTESIAN_POINT ( 'NONE',  ( 0.1749999999999999889, 8.800000000000000711, 0.4000000000000000222 ) ) ;
#18087 = CARTESIAN_POINT ( 'NONE',  ( 0.1749999999999999889, 7.900000000000000355, 0.5999999999999999778 ) ) ;
#18088 = EDGE_LOOP ( 'NONE', ( #11188, #9962, #15365, #5659 ) ) ;
#18089 = CARTESIAN_POINT ( 'NONE',  ( -2.306642602145299925, -5.515466101694909362, 5.166805192608490138 ) ) ;
#18090 = CARTESIAN_POINT ( 'NONE',  ( -0.3162622016569221484, -4.245794312053864594, 7.334974746141788238 ) ) ;
#18091 = CARTESIAN_POINT ( 'NONE',  ( -2.574214976178951009, -3.403575057315514130, 4.054607910322786779 ) ) ;
#18092 = PLANE ( 'NONE',  #17358 ) ;
#18093 = EDGE_CURVE ( 'NONE', #1995, #12906, #6215, .T. ) ;
#18094 = CARTESIAN_POINT ( 'NONE',  ( 1.458615186838411626, -0.4963798976394455664, 3.259477383973563125 ) ) ;
#18096 = EDGE_CURVE ( 'NONE', #10706, #5909, #6383, .T. ) ;
#18095 = CARTESIAN_POINT ( 'NONE',  ( -1.800000000000000044, 0.5999999999999999778, 7.599999999999999645 ) ) ;
#18097 = ORIENTED_EDGE ( 'NONE', *, *, #12782, .F. ) ;
#18098 = CARTESIAN_POINT ( 'NONE',  ( 0.1749999999999999889, 9.299999999999998934, 1.600000000000000089 ) ) ;
#18099 = CARTESIAN_POINT ( 'NONE',  ( -1.925796468768790071, -0.4957627118644070130, 6.052706598917719560 ) ) ;
#18100 = CARTESIAN_POINT ( 'NONE',  ( -1.948278411993560111, -3.193980462720909852, 6.020210936496040333 ) ) ;
#18101 = DIRECTION ( 'NONE',  ( 1.000000000000000000, 0.000000000000000000, -7.401486830834370362E-16 ) ) ;
#18102 = DIRECTION ( 'NONE',  ( 2.220446049250309876E-16, 1.000000000000000000, -1.064962222048364037E-31 ) ) ;
#18103 = CARTESIAN_POINT ( 'NONE',  ( 0.7998959936908462964, -5.435381355932195291, 7.230419212249866945 ) ) ;
#18104 = ORIENTED_EDGE ( 'NONE', *, *, #7129, .F. ) ;
#18105 = FACE_OUTER_BOUND ( 'NONE', #1397, .T. ) ;
#18106 = DIRECTION ( 'NONE',  ( 0.7071067811865475727, 4.617918996128745560E-17, 0.7071067811865475727 ) ) ;
#18107 = DIRECTION ( 'NONE',  ( 3.097720492815730124E-16, 1.000000000000000000, 0.000000000000000000 ) ) ;
#18108 = CARTESIAN_POINT ( 'NONE',  ( -2.500000000000000000, 1.071484571201660082E-16, -8.514390157257050626E-16 ) ) ;
#18109 = ORIENTED_EDGE ( 'NONE', *, *, #1896, .T. ) ;
#18110 = CARTESIAN_POINT ( 'NONE',  ( 1.994983296312400123, -4.265241723982169830, 5.948514050749290405 ) ) ;
#18111 = CARTESIAN_POINT ( 'NONE',  ( 0.8534102632286154622, -5.320452325212860600, 2.829778315381550780 ) ) ;
#18112 = DIRECTION ( 'NONE',  ( 0.000000000000000000, 1.000000000000000000, 0.000000000000000000 ) ) ;
#18114 = EDGE_CURVE ( 'NONE', #16120, #8561, #15643, .T. ) ;
#18113 = CARTESIAN_POINT ( 'NONE',  ( 0.5000000000000000000, 3.500000000000000000, 6.100000000000000533 ) ) ;
#18115 = CARTESIAN_POINT ( 'NONE',  ( -2.219956784870669608, -3.426863345603790023, 3.918630970161619764 ) ) ;
#18116 = FACE_OUTER_BOUND ( 'NONE', #17, .T. ) ;
#18117 = CARTESIAN_POINT ( 'NONE',  ( -0.8259795455965642796, -3.054250732991181216, 6.579537079411896805 ) ) ;
#18118 = DIRECTION ( 'NONE',  ( 1.000000000000000000, 0.000000000000000000, 0.000000000000000000 ) ) ;
#18119 = CARTESIAN_POINT ( 'NONE',  ( -0.1471036068827911436, -0.2965485159365571777, 2.649244128781490737 ) ) ;
#18120 = ORIENTED_EDGE ( 'NONE', *, *, #6072, .T. ) ;
#18121 = DIRECTION ( 'NONE',  ( 1.470526319674639030E-16, 0.7492686492653546360, -0.6622661785325225647 ) ) ;
#18122 = ORIENTED_EDGE ( 'NONE', *, *, #15801, .F. ) ;
#18123 = ORIENTED_EDGE ( 'NONE', *, *, #10412, .F. ) ;
#18124 = VERTEX_POINT ( 'NONE', #4633 ) ;
#18125 = CARTESIAN_POINT ( 'NONE',  ( -0.1749999999999999889, 9.299999999999998934, 1.600000000000000089 ) ) ;
#18126 = COLOUR_RGB ( '', 0.66274510, 0.83137255, 0.94901961) ;
#18127 = CARTESIAN_POINT ( 'NONE',  ( -1.351903350398179438, -5.184322033898315141, 6.245004350000422200 ) ) ;
#18128 = CARTESIAN_POINT ( 'NONE',  ( 1.800000000000000044, 12.00000000000000000, 1.600000000000000089 ) ) ;
#18129 = DIRECTION ( 'NONE',  ( 0.9396926207859082059, 0.000000000000000000, -0.3420201433256691015 ) ) ;
#18130 = DIRECTION ( 'NONE',  ( 1.216682766712499758E-16, 4.229421046191059358E-17, 1.000000000000000000 ) ) ;
#18131 = DIRECTION ( 'NONE',  ( 7.401486830834370362E-16, 0.000000000000000000, 1.000000000000000000 ) ) ;
#18132 = CARTESIAN_POINT ( 'NONE',  ( -2.500000000000000000, 2.000000000000000000, -2.537652627714639929E-16 ) ) ;
#18133 = CARTESIAN_POINT ( 'NONE',  ( -2.005512128484160161, -1.913124606865060029, 3.468469736471389897 ) ) ;
#18134 = CARTESIAN_POINT ( 'NONE',  ( 0.07299321914061039640, -0.001483050847457899942, 2.350000000000000089 ) ) ;
#18135 = ORIENTED_EDGE ( 'NONE', *, *, #2275, .T. ) ;
#18136 = CARTESIAN_POINT ( 'NONE',  ( 2.345900685764729765, -0.3711864406779670222, 4.512231114381330066 ) ) ;
#18137 = CARTESIAN_POINT ( 'NONE',  ( 2.306642602145299925, -0.3845338983050849979, 5.166805192608480368 ) ) ;
#18138 = ORIENTED_EDGE ( 'NONE', *, *, #14042, .F. ) ;
#18139 = CARTESIAN_POINT ( 'NONE',  ( 1.246151616534670215, -0.03114406779661053892, 3.068501529594759081 ) ) ;
#18140 = DIRECTION ( 'NONE',  ( 9.796085511398438540E-17, -1.000000000000000000, 0.000000000000000000 ) ) ;
#18141 = ORIENTED_EDGE ( 'NONE', *, *, #17493, .T. ) ;
#18142 = DIRECTION ( 'NONE',  ( -1.000000000000000000, 0.000000000000000000, 0.000000000000000000 ) ) ;
#18143 = CARTESIAN_POINT ( 'NONE',  ( -1.832842064134659665, -2.871785303044850579, 6.176291182464519913 ) ) ;
#18144 = DIRECTION ( 'NONE',  ( 1.000000000000000000, 0.000000000000000000, 0.000000000000000000 ) ) ;
#18145 = CARTESIAN_POINT ( 'NONE',  ( -1.747582379783008788, -5.484322033898315851, 6.697200745122486865 ) ) ;
#18146 = EDGE_CURVE ( 'NONE', #15707, #2630, #18273, .T. ) ;
#18147 = EDGE_LOOP ( 'NONE', ( #10156, #4911, #11723 ) ) ;
#18148 = CARTESIAN_POINT ( 'NONE',  ( -2.091095264232510242, -1.656953435693890198, 5.779845490516250628 ) ) ;
#18149 = EDGE_CURVE ( 'NONE', #12817, #4099, #10556, .T. ) ;
#18150 = CARTESIAN_POINT ( 'NONE',  ( -1.134881315981510541, -0.4779661016949154906, 6.410767520434657918 ) ) ;
#18151 = ORIENTED_EDGE ( 'NONE', *, *, #3688, .F. ) ;
#18152 = FACE_OUTER_BOUND ( 'NONE', #634, .T. ) ;
#18153 = CARTESIAN_POINT ( 'NONE',  ( 2.500000000000000000, 11.29999999999999893, 7.649999999999999467 ) ) ;
#18154 = CARTESIAN_POINT ( 'NONE',  ( 2.500000000000000000, 0.7500000000000000000, 7.649999999999999467 ) ) ;
#18155 = CARTESIAN_POINT ( 'NONE',  ( 1.688800633088581860, -0.8418633456037974971, 3.532586505616389871 ) ) ;
#18156 = CARTESIAN_POINT ( 'NONE',  ( 2.500000000000000000, 4.700000000000000178, 1.600000000000000089 ) ) ;
#18157 = ORIENTED_EDGE ( 'NONE', *, *, #14466, .T. ) ;
#18158 = DIRECTION ( 'NONE',  ( -1.853875224168160112E-15, -1.000000000000000000, -2.960594732333760372E-15 ) ) ;
#18159 = DIRECTION ( 'NONE',  ( -0.000000000000000000, 1.000000000000000000, 0.000000000000000000 ) ) ;
#18160 = CARTESIAN_POINT ( 'NONE',  ( 1.921786527979010062, -0.3578389830508479363, 3.977907449687776431 ) ) ;
#18161 = CARTESIAN_POINT ( 'NONE',  ( 1.132648842710480830, -4.106064582324130185, 7.100045893750476900 ) ) ;
#18162 = CARTESIAN_POINT ( 'NONE',  ( -1.053623506755599459, -4.865515740159335856, 2.921978671571880515 ) ) ;
#18163 = CARTESIAN_POINT ( 'NONE',  ( 1.494593880360790550, -5.338983050847455836, 3.295456077495951153 ) ) ;
#18164 = VERTEX_POINT ( 'NONE', #14926 ) ;
#18165 = EDGE_CURVE ( 'NONE', #6674, #12720, #3263, .T. ) ;
#18166 = CARTESIAN_POINT ( 'NONE',  ( 1.438959988998139914E-16, 0.000000000000000000, 2.350000000000000089 ) ) ;
#18167 = DIRECTION ( 'NONE',  ( 1.000000000000000000, -1.103950578158349959E-14, 0.000000000000000000 ) ) ;
#18168 = CARTESIAN_POINT ( 'NONE',  ( -1.377628188826471423, -0.5741044150835525883, 2.411088859383701433 ) ) ;
#18169 = EDGE_CURVE ( 'NONE', #16021, #12172, #16042, .T. ) ;
#18170 = ORIENTED_EDGE ( 'NONE', *, *, #4848, .F. ) ;
#18171 = CARTESIAN_POINT ( 'NONE',  ( -2.340070819011249803, -5.519915254237290014, 4.950151441910549899 ) ) ;
#18172 = EDGE_CURVE ( 'NONE', #1173, #10172, #11873, .T. ) ;
#18173 = CARTESIAN_POINT ( 'NONE',  ( 2.235075160050071119, -3.966334852594401994, 6.130927224539736820 ) ) ;
#18174 = EDGE_CURVE ( 'NONE', #12759, #7292, #2009, .T. ) ;
#18175 = DIRECTION ( 'NONE',  ( 0.000000000000000000, 0.000000000000000000, -1.000000000000000000 ) ) ;
#18176 = CARTESIAN_POINT ( 'NONE',  ( -1.835037444103819970, -1.358046564306109261, 5.620619042473610882 ) ) ;
#18177 = VECTOR ( 'NONE', #7913, 1000.000000000000000 ) ;
#18178 = CARTESIAN_POINT ( 'NONE',  ( -1.800000000000000044, 7.799999999999999822, 7.599999999999999645 ) ) ;
#18179 = ORIENTED_EDGE ( 'NONE', *, *, #12544, .T. ) ;
#18180 = CARTESIAN_POINT ( 'NONE',  ( -1.899999999999999911, 2.799999999999999822, 1.600000000000000089 ) ) ;
#18181 = CARTESIAN_POINT ( 'NONE',  ( 1.851073041990159984, -0.4067796610169499560, 6.153284478378259870 ) ) ;
#18182 = CARTESIAN_POINT ( 'NONE',  ( 1.353103843060669886, -2.798079561820010053, 6.625579309552930063 ) ) ;
#18183 = DIRECTION ( 'NONE',  ( 2.220446049250309876E-16, 1.000000000000000000, 0.000000000000000000 ) ) ;
#18184 = CARTESIAN_POINT ( 'NONE',  ( -1.149999999999999911, 9.248236190979499227, 7.693185165257809821 ) ) ;
#18185 = CARTESIAN_POINT ( 'NONE',  ( 2.578017356471871135, -5.086440677966105994, 5.329826563567761077 ) ) ;
#18186 = EDGE_LOOP ( 'NONE', ( #9310, #6384, #7498, #5495 ) ) ;
#18187 = CIRCLE ( 'NONE', #2251, 0.4166666666666671848 ) ;
#18188 = ORIENTED_EDGE ( 'NONE', *, *, #5878, .T. ) ;
#18189 = DIRECTION ( 'NONE',  ( 1.000000000000000000, 0.000000000000000000, -6.049014748177260544E-16 ) ) ;
#18190 = CARTESIAN_POINT ( 'NONE',  ( -1.800000000000000044, 11.29999999999999893, 1.600000000000000089 ) ) ;
#18191 = CARTESIAN_POINT ( 'NONE',  ( -1.800000000000000044, 11.40000000000000036, 6.599999999999999645 ) ) ;
#18192 = EDGE_CURVE ( 'NONE', #14967, #9046, #12378, .T. ) ;
#18193 = ORIENTED_EDGE ( 'NONE', *, *, #6878, .F. ) ;
#18194 = VECTOR ( 'NONE', #7726, 1000.000000000000000 ) ;
#18195 = CARTESIAN_POINT ( 'NONE',  ( -2.334032080503389839, -3.310421904162350160, 5.001728246382240783 ) ) ;
#18196 = CARTESIAN_POINT ( 'NONE',  ( 1.875000000000000000, 11.25000000000000000, 7.700000000000000178 ) ) ;
#18197 = CARTESIAN_POINT ( 'NONE',  ( 0.9788656693287738353, -5.320452325212859712, 2.556357798777459944 ) ) ;
#18198 = DIRECTION ( 'NONE',  ( 1.000000000000000000, -1.850371707708589879E-16, 0.000000000000000000 ) ) ;
#18199 = DIRECTION ( 'NONE',  ( -7.109522442527898025E-16, 0.000000000000000000, -1.000000000000000000 ) ) ;
#18200 = CARTESIAN_POINT ( 'NONE',  ( 1.026235786675480099, -4.404971453711899798, 6.817920158464540137 ) ) ;
#18201 = DIRECTION ( 'NONE',  ( 0.000000000000000000, 0.000000000000000000, -1.000000000000000000 ) ) ;
#18202 = CARTESIAN_POINT ( 'NONE',  ( 1.800000000000000044, 12.00000000000000000, 7.649999999999999467 ) ) ;
#18203 = CARTESIAN_POINT ( 'NONE',  ( 0.2993653819235879698, -2.914521003261450360, 6.731079075450741911 ) ) ;
#18204 = AXIS2_PLACEMENT_3D ( 'NONE', #14759, #15061, #2370 ) ;
#18205 = EDGE_CURVE ( 'NONE', #7679, #4501, #16217, .T. ) ;
#18206 = CARTESIAN_POINT ( 'NONE',  ( 0.4000000000000000222, -1.399999999999999911, 5.100000000000000533 ) ) ;
#18207 = CIRCLE ( 'NONE', #10240, 0.4000000000000000222 ) ;
#18208 = EDGE_LOOP ( 'NONE', ( #16937, #14346 ) ) ;
#18209 = CARTESIAN_POINT ( 'NONE',  ( -0.009452110982655708218, -0.5998079552954630467, 2.350000000000000089 ) ) ;
#18210 = ORIENTED_EDGE ( 'NONE', *, *, #3519, .F. ) ;
#18211 = LINE ( 'NONE', #10009, #15787 ) ;
#18212 = ADVANCED_FACE ( 'NONE', ( #4812 ), #14831, .F. ) ;
#18213 = ORIENTED_EDGE ( 'NONE', *, *, #14564, .T. ) ;
#18214 = ORIENTED_EDGE ( 'NONE', *, *, #10288, .F. ) ;
#18215 = VECTOR ( 'NONE', #8400, 1000.000000000000000 ) ;
#18216 = EDGE_CURVE ( 'NONE', #17934, #16120, #16311, .T. ) ;
#18217 = ORIENTED_EDGE ( 'NONE', *, *, #7463, .T. ) ;
#18218 = CARTESIAN_POINT ( 'NONE',  ( -0.9000000000000000222, 2.050000000000000266, 3.600000000000000089 ) ) ;
#18219 = CARTESIAN_POINT ( 'NONE',  ( -1.246151616534680651, -5.268855932203385883, 3.068501529594771071 ) ) ;
#18220 = CARTESIAN_POINT ( 'NONE',  ( -2.470260739716218179, -1.567641158900710430, 3.729986819255259878 ) ) ;
#18221 = VECTOR ( 'NONE', #1273, 1000.000000000000000 ) ;
#18222 = DIRECTION ( 'NONE',  ( 1.224646799147349016E-16, 0.000000000000000000, 1.000000000000000000 ) ) ;
#18223 = AXIS2_PLACEMENT_3D ( 'NONE', #13788, #3970, #16664 ) ;
#18224 = PLANE ( 'NONE',  #7311 ) ;
#18225 = DIRECTION ( 'NONE',  ( 0.000000000000000000, -1.000000000000000000, 0.000000000000000000 ) ) ;
#18226 = FACE_OUTER_BOUND ( 'NONE', #15927, .T. ) ;
#18227 = DIRECTION ( 'NONE',  ( -0.000000000000000000, 1.000000000000000000, 0.000000000000000000 ) ) ;
#18228 = CARTESIAN_POINT ( 'NONE',  ( 1.902324933209389890, -2.402178660919109809, 3.314393441133530072 ) ) ;
#18229 = VECTOR ( 'NONE', #15218, 1000.000000000000000 ) ;
#18230 = DIRECTION ( 'NONE',  ( 1.000000000000000000, 0.000000000000000000, 0.000000000000000000 ) ) ;
#18231 = VECTOR ( 'NONE', #7994, 1000.000000000000000 ) ;
#18232 = CARTESIAN_POINT ( 'NONE',  ( -2.048006021857541548, -3.058091609351150986, 4.556566471620694614 ) ) ;
#18233 = AXIS2_PLACEMENT_3D ( 'NONE', #6483, #11946, #14916 ) ;
#18234 = CARTESIAN_POINT ( 'NONE',  ( -1.925796468768790071, -0.1957627118644069963, 6.052706598917719560 ) ) ;
#18235 = CARTESIAN_POINT ( 'NONE',  ( 1.800000000000000044, 11.40000000000000036, 1.600000000000000089 ) ) ;
#18236 = LINE ( 'NONE', #9844, #14483 ) ;
#18237 = ORIENTED_EDGE ( 'NONE', *, *, #9005, .F. ) ;
#18238 = VECTOR ( 'NONE', #5980, 1000.000000000000000 ) ;
#18239 = CARTESIAN_POINT ( 'NONE',  ( -0.7093417302541390468, -0.1646186440677969987, 6.943956659919700236 ) ) ;
#18240 = VECTOR ( 'NONE', #16363, 1000.000000000000000 ) ;
#18241 = CARTESIAN_POINT ( 'NONE',  ( -1.399999999999999911, -5.000000000000000000, 6.100000000000000533 ) ) ;
#18242 = ORIENTED_EDGE ( 'NONE', *, *, #17102, .T. ) ;
#18243 = DIRECTION ( 'NONE',  ( 0.000000000000000000, 0.000000000000000000, -1.000000000000000000 ) ) ;
#18244 = VERTEX_POINT ( 'NONE', #9266 ) ;
#18245 = CARTESIAN_POINT ( 'NONE',  ( -2.190084968185499914, -1.567641158900710208, 3.838447030292489348 ) ) ;
#18246 = CARTESIAN_POINT ( 'NONE',  ( -3.408368997776849933E-15, -5.599999999999999645, 2.350000000000000089 ) ) ;
#18247 = AXIS2_PLACEMENT_3D ( 'NONE', #17840, #9537, #16841 ) ;
#18248 = AXIS2_PLACEMENT_3D ( 'NONE', #1565, #271, #5729 ) ;
#18249 = ORIENTED_EDGE ( 'NONE', *, *, #7236, .T. ) ;
#18250 = CARTESIAN_POINT ( 'NONE',  ( 2.287919158821199783, -1.051457940198389895, 5.251517552016890633 ) ) ;
#18251 = CARTESIAN_POINT ( 'NONE',  ( -1.562863241354461641, -0.4913135593220345210, 6.031217337312382298 ) ) ;
#18252 = ADVANCED_FACE ( 'NONE', ( #6121 ), #11785, .T. ) ;
#18253 = VERTEX_POINT ( 'NONE', #16924 ) ;
#18254 = VECTOR ( 'NONE', #2273, 1000.000000000000000 ) ;
#18255 = ADVANCED_FACE ( 'NONE', ( #12239 ), #7031, .T. ) ;
#18256 = CARTESIAN_POINT ( 'NONE',  ( 1.300000000000000044, -1.592040838891560081E-16, 7.599999999999999645 ) ) ;
#18257 = CARTESIAN_POINT ( 'NONE',  ( -1.000000000000000000, -6.000000000000000000, 3.299999999999999822 ) ) ;
#18258 = DIRECTION ( 'NONE',  ( 1.216682766712499758E-16, 4.229421046191059358E-17, 1.000000000000000000 ) ) ;
#18259 = CARTESIAN_POINT ( 'NONE',  ( -1.485933537025771356, -4.796950468210009255, 3.286232459959995911 ) ) ;
#18260 = CARTESIAN_POINT ( 'NONE',  ( -0.1749999999999999889, 9.299999999999998934, 1.600000000000000089 ) ) ;
#18261 = ORIENTED_EDGE ( 'NONE', *, *, #10281, .F. ) ;
#18262 = CYLINDRICAL_SURFACE ( 'NONE', #9842, 1.016666666666670160 ) ;
#18263 = AXIS2_PLACEMENT_3D ( 'NONE', #5264, #6458, #6267 ) ;
#18264 = DIRECTION ( 'NONE',  ( 6.123233995736764803E-17, -1.000000000000000000, 0.000000000000000000 ) ) ;
#18265 = COLOUR_RGB ( '', 0.66274510, 0.83137255, 0.94901961) ;
#18266 = CARTESIAN_POINT ( 'NONE',  ( -1.580445181003969912, -0.2580508474576271305, 3.389704561770339630 ) ) ;
#18267 = CARTESIAN_POINT ( 'NONE',  ( 0.6672256841321406728, -4.152641158900696183, 7.268642361138727637 ) ) ;
#18268 = ADVANCED_FACE ( 'NONE', ( #1286 ), #5728, .T. ) ;
#18269 = DIRECTION ( 'NONE',  ( -1.000000000000000000, 0.000000000000000000, 0.000000000000000000 ) ) ;
#18270 = CARTESIAN_POINT ( 'NONE',  ( -0.5230055860628765041, -5.251463457376924104, 2.087624054227240844 ) ) ;
#18271 = CARTESIAN_POINT ( 'NONE',  ( -1.614765845140348821, -5.193220338983044471, 5.967758800287426446 ) ) ;
#18272 = ORIENTED_EDGE ( 'NONE', *, *, #14600, .T. ) ;
#18273 = CIRCLE ( 'NONE', #15351, 0.5000000000000000000 ) ;
#18274 = FACE_OUTER_BOUND ( 'NONE', #7862, .T. ) ;
#18275 = FACE_OUTER_BOUND ( 'NONE', #3013, .T. ) ;
#18276 = CARTESIAN_POINT ( 'NONE',  ( -0.1869574461324000070, -0.5962015548080630278, 2.350675676344399889 ) ) ;
#18277 = ORIENTED_EDGE ( 'NONE', *, *, #11553, .F. ) ;
#18278 = CARTESIAN_POINT ( 'NONE',  ( 1.899999999999999911, 7.299999999999999822, 1.600000000000000089 ) ) ;
#18279 = VECTOR ( 'NONE', #8855, 1000.000000000000000 ) ;
#18280 = VECTOR ( 'NONE', #15682, 1000.000000000000000 ) ;
#18281 = CARTESIAN_POINT ( 'NONE',  ( -0.3949552299395130417, -1.823812330071880039, 2.379923265530350385 ) ) ;
#18282 = EDGE_CURVE ( 'NONE', #15780, #13146, #9108, .T. ) ;
#18283 = CARTESIAN_POINT ( 'NONE',  ( 1.899999999999999911, 2.799999999999999822, 0.5999999999999999778 ) ) ;
#18284 = CARTESIAN_POINT ( 'NONE',  ( -2.016543577558690625, -1.521064582324129777, 4.314702916654059806 ) ) ;
#18285 = CARTESIAN_POINT ( 'NONE',  ( -1.800000000000000044, 0.5999999999999999778, 1.600000000000000089 ) ) ;
#18286 = VECTOR ( 'NONE', #946, 1000.000000000000000 ) ;
#18287 = EDGE_CURVE ( 'NONE', #4545, #8308, #14052, .T. ) ;
#18288 = ORIENTED_EDGE ( 'NONE', *, *, #11975, .T. ) ;
#18289 = EDGE_CURVE ( 'NONE', #2568, #10948, #11284, .T. ) ;
#18290 = CARTESIAN_POINT ( 'NONE',  ( -1.000000000000000000, -8.000000000000000000, 5.700000000000000178 ) ) ;
#18291 = DIRECTION ( 'NONE',  ( 1.168655815394900078E-16, -1.000000000000000000, 0.000000000000000000 ) ) ;
#18292 = NEXT_ASSEMBLY_USAGE_OCCURRENCE ( 'NAUO1', ' ', ' ', #17933, #4382, $ ) ;
#18293 = NEXT_ASSEMBLY_USAGE_OCCURRENCE ( 'NAUO2', ' ', ' ', #17933, #7122, $ ) ;
#18294 = NEXT_ASSEMBLY_USAGE_OCCURRENCE ( 'NAUO3', ' ', ' ', #17933, #14462, $ ) ;
#18295 = NEXT_ASSEMBLY_USAGE_OCCURRENCE ( 'NAUO4', ' ', ' ', #17933, #15932, $ ) ;
#18296 = NEXT_ASSEMBLY_USAGE_OCCURRENCE ( 'NAUO5', ' ', ' ', #17933, #3578, $ ) ;
#18297 = NEXT_ASSEMBLY_USAGE_OCCURRENCE ( 'NAUO6', ' ', ' ', #17933, #12313, $ ) ;
#18298 = NEXT_ASSEMBLY_USAGE_OCCURRENCE ( 'NAUO7', ' ', ' ', #17933, #2227, $ ) ;
#18299 = NEXT_ASSEMBLY_USAGE_OCCURRENCE ( 'NAUO8', ' ', ' ', #17933, #15039, $ ) ;
#18300 = NEXT_ASSEMBLY_USAGE_OCCURRENCE ( 'NAUO9', ' ', ' ', #17933, #13304, $ ) ;
#18301 = NEXT_ASSEMBLY_USAGE_OCCURRENCE ( 'NAUO10', ' ', ' ', #17933, #14462, $ ) ;
#18302 = NEXT_ASSEMBLY_USAGE_OCCURRENCE ( 'NAUO11', ' ', ' ', #17933, #14462, $ ) ;
ENDSEC;
END-ISO-10303-21;
